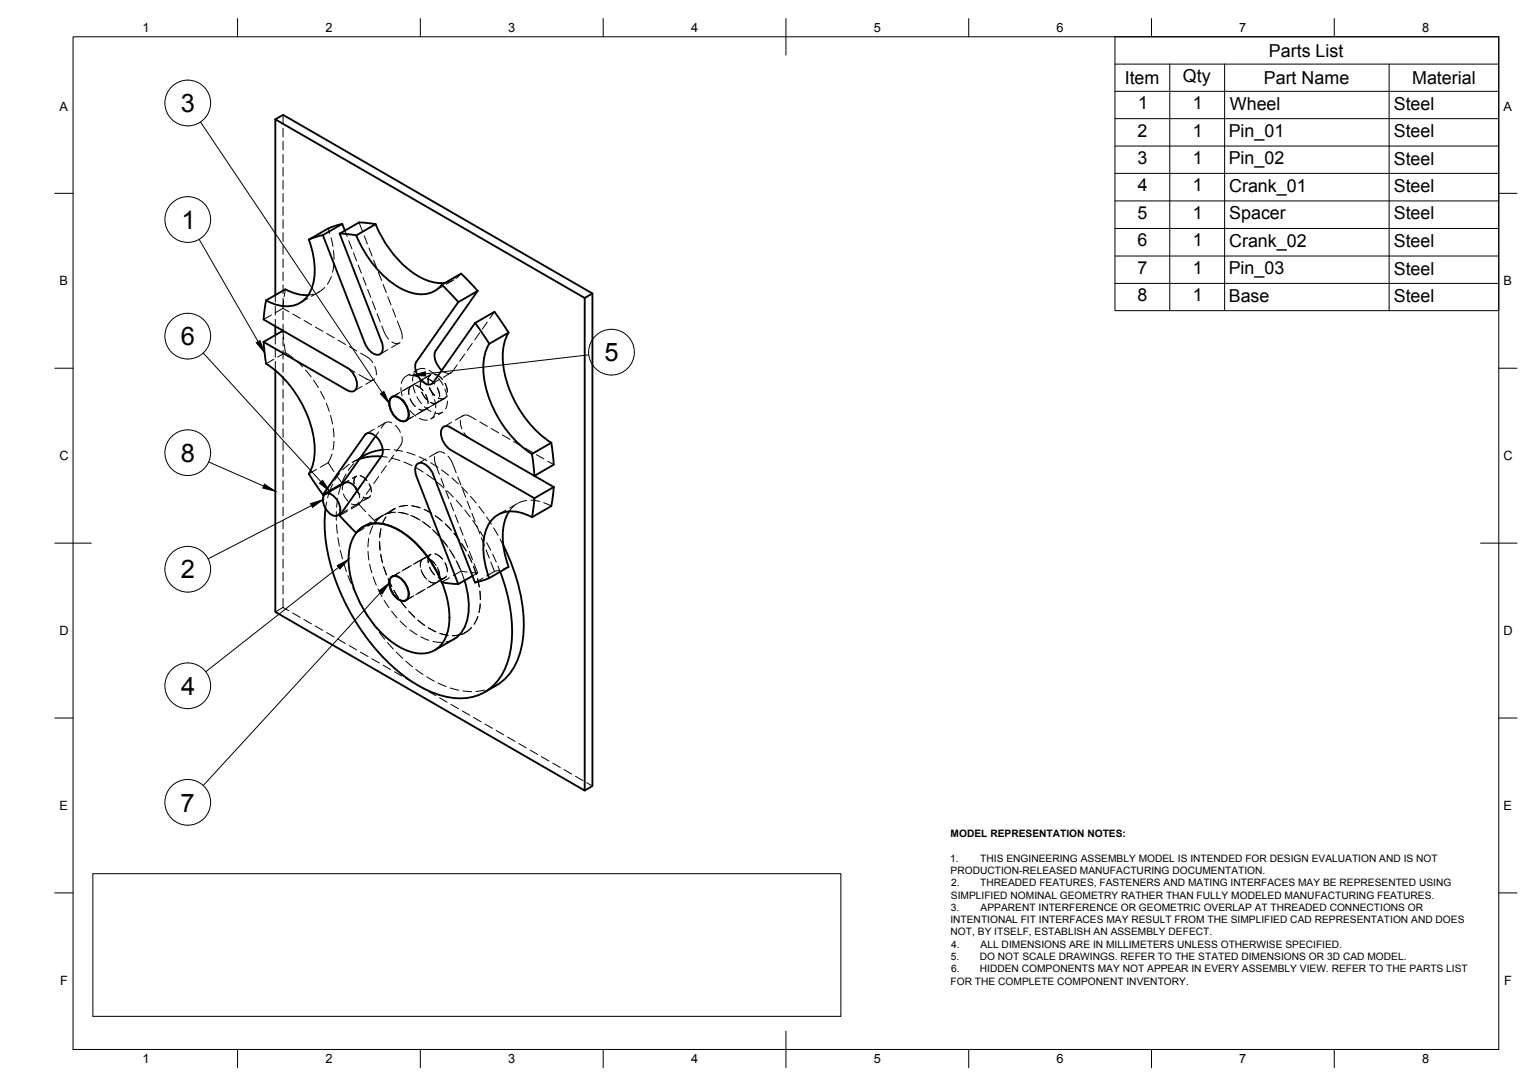
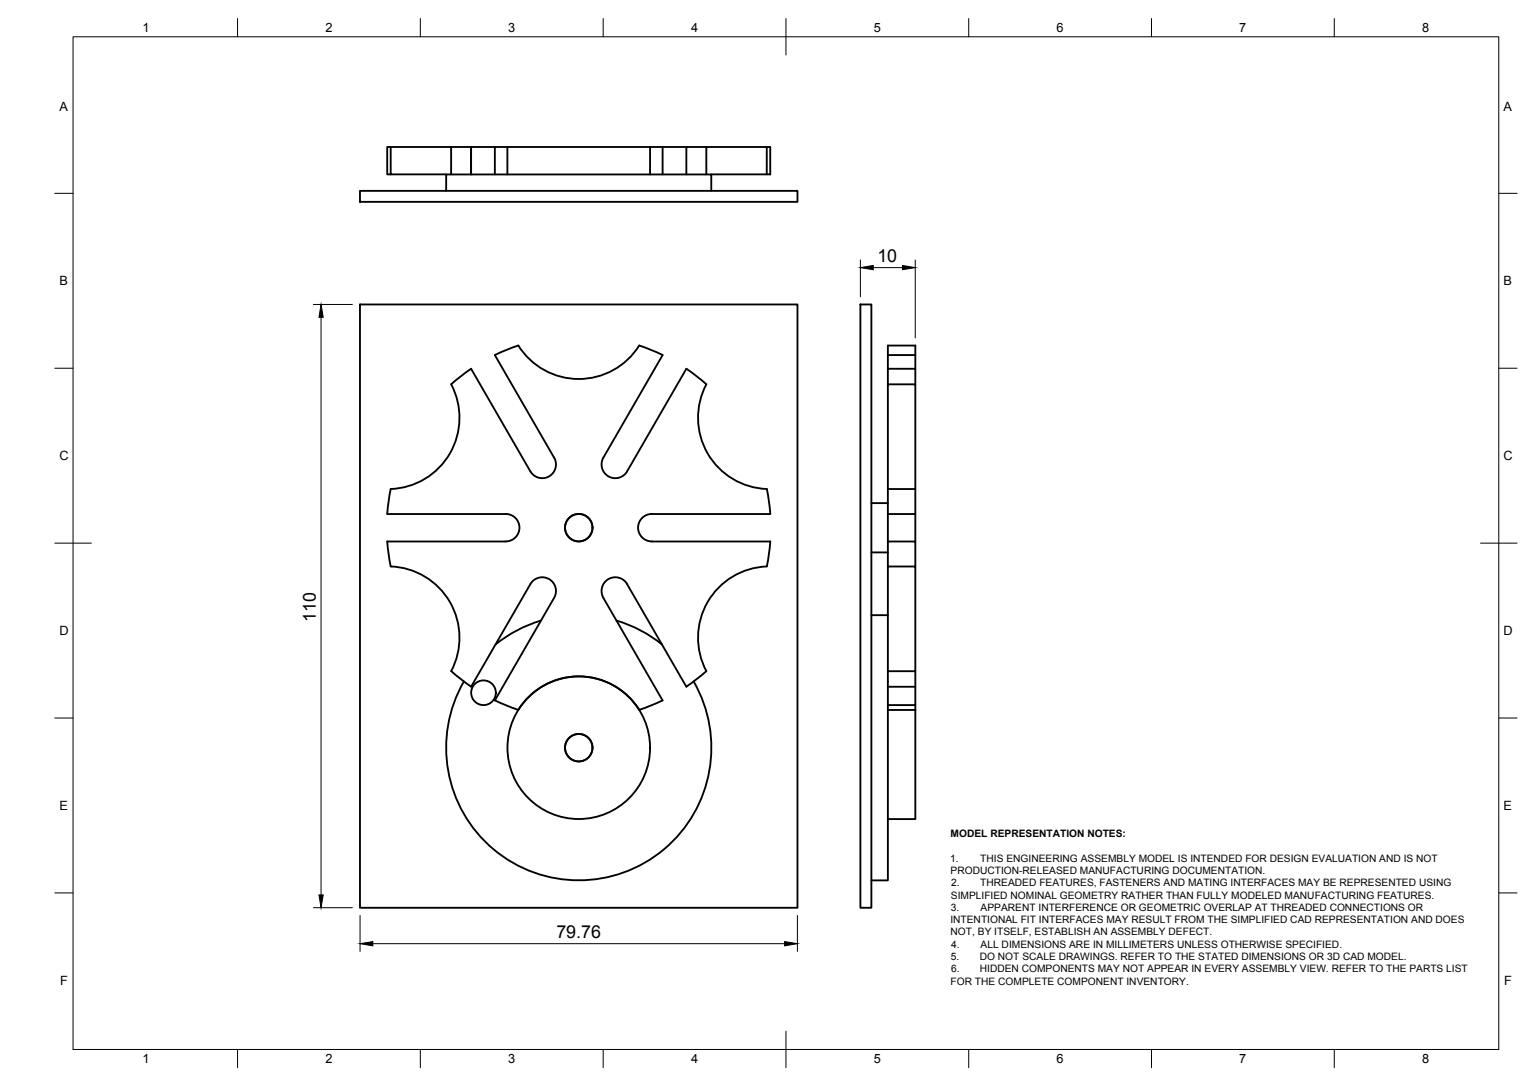
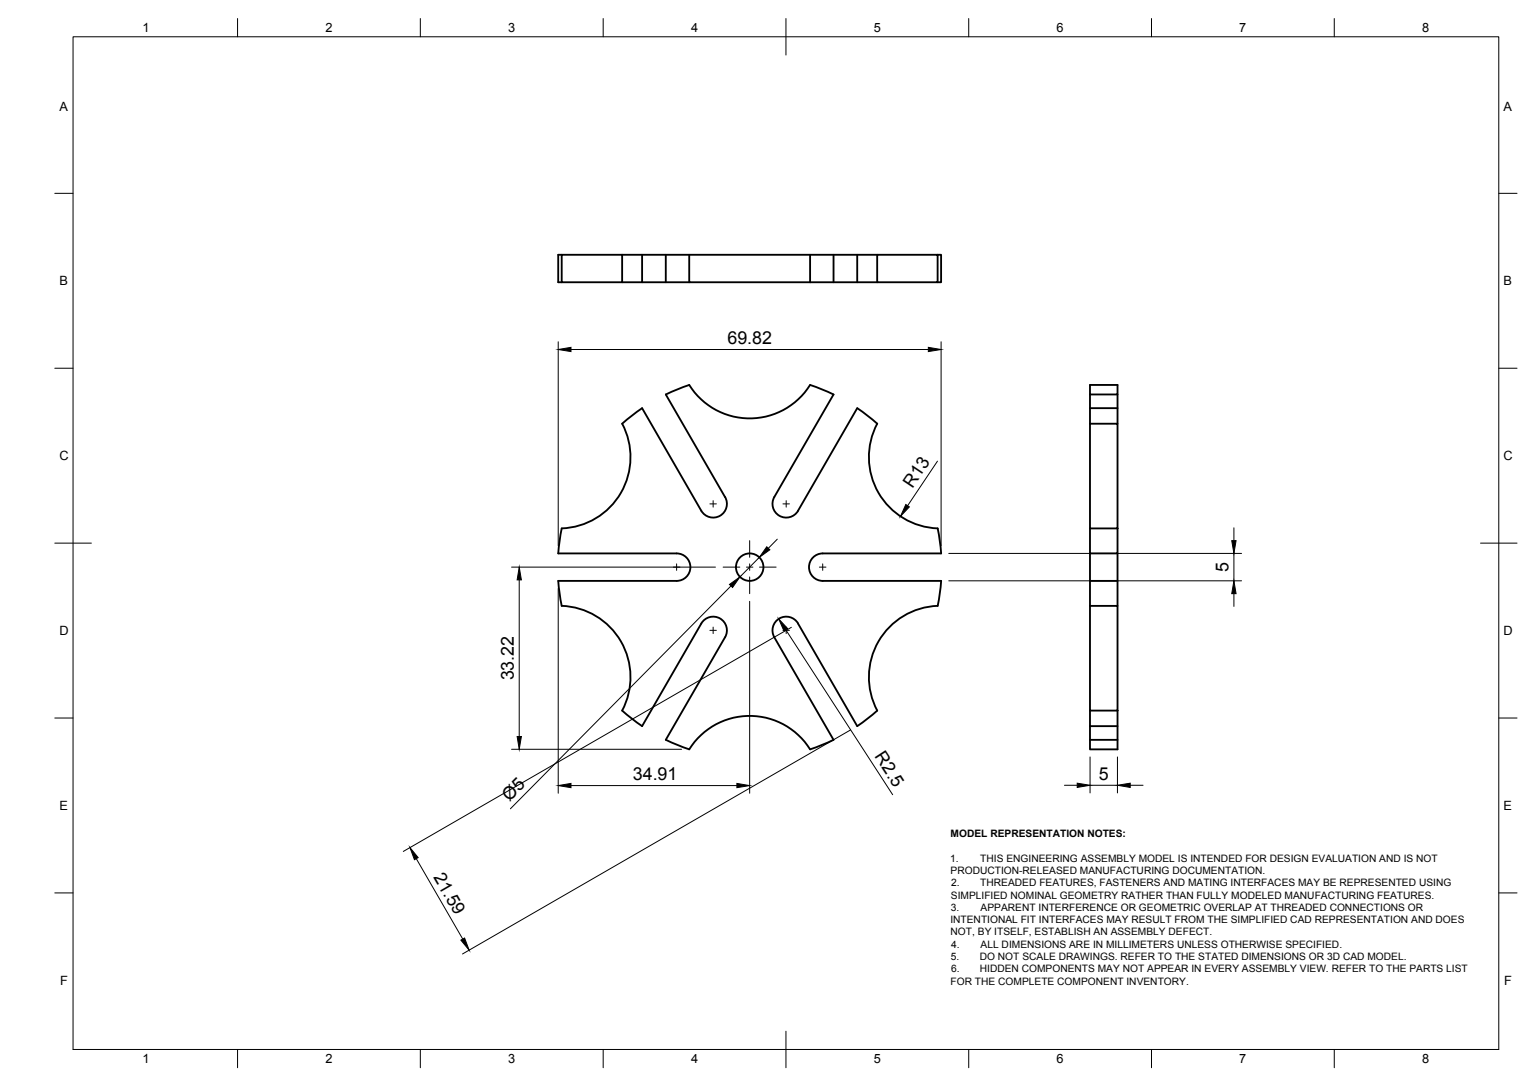
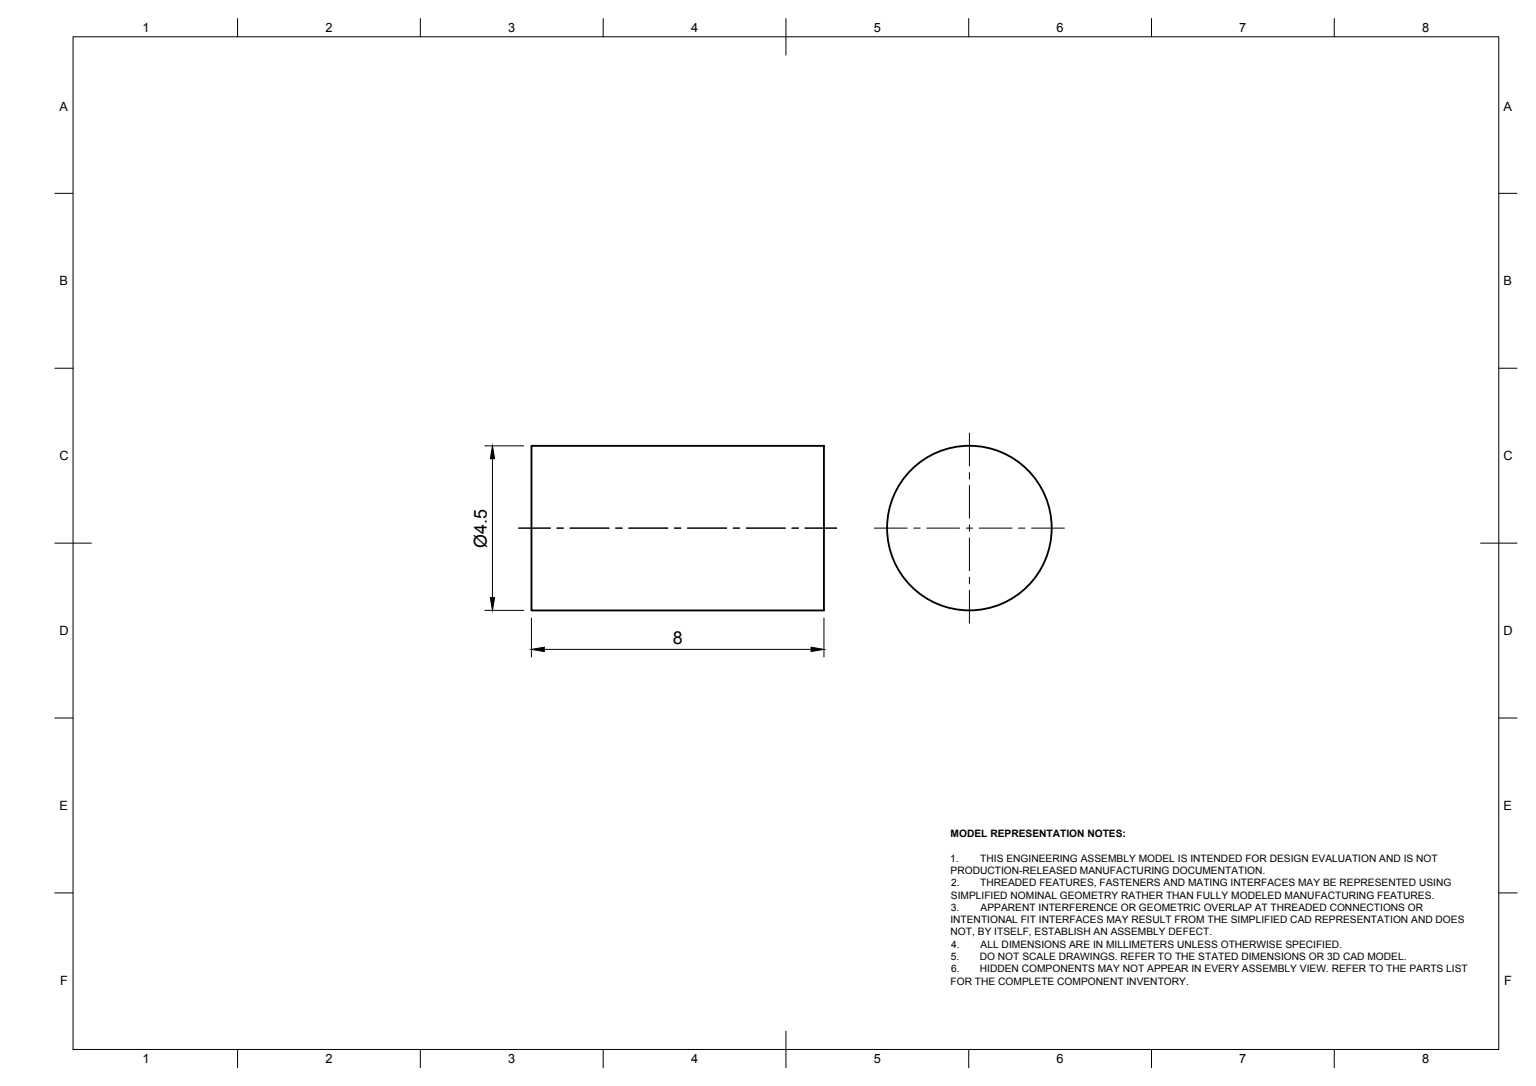
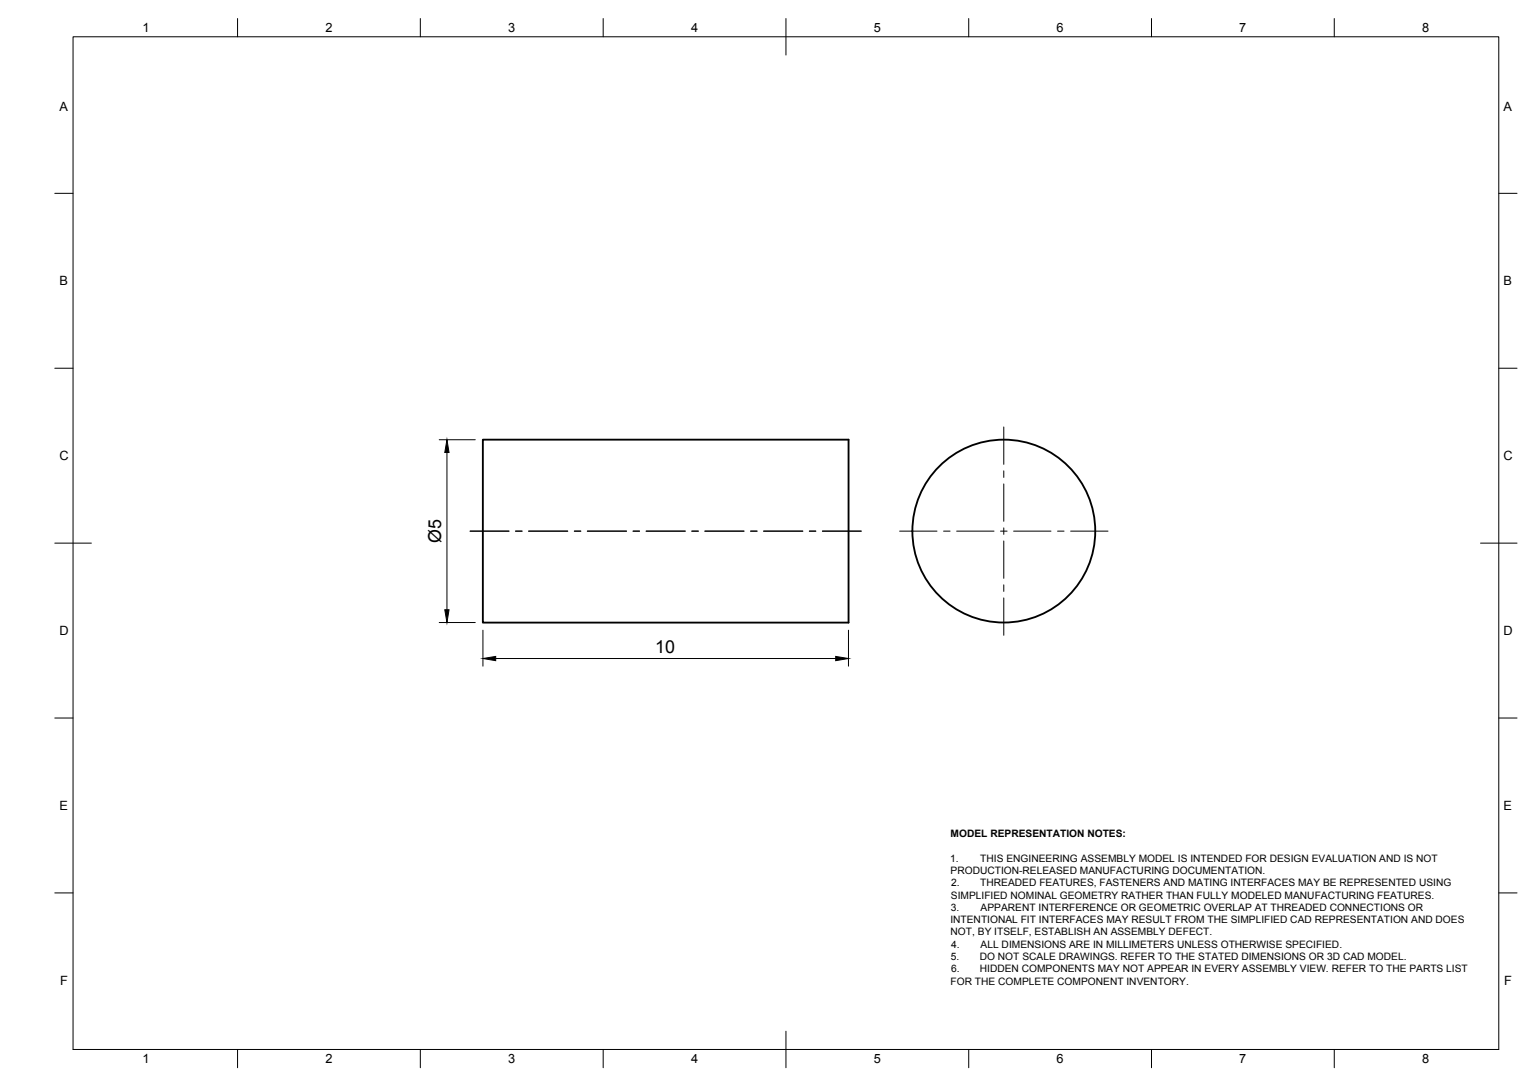
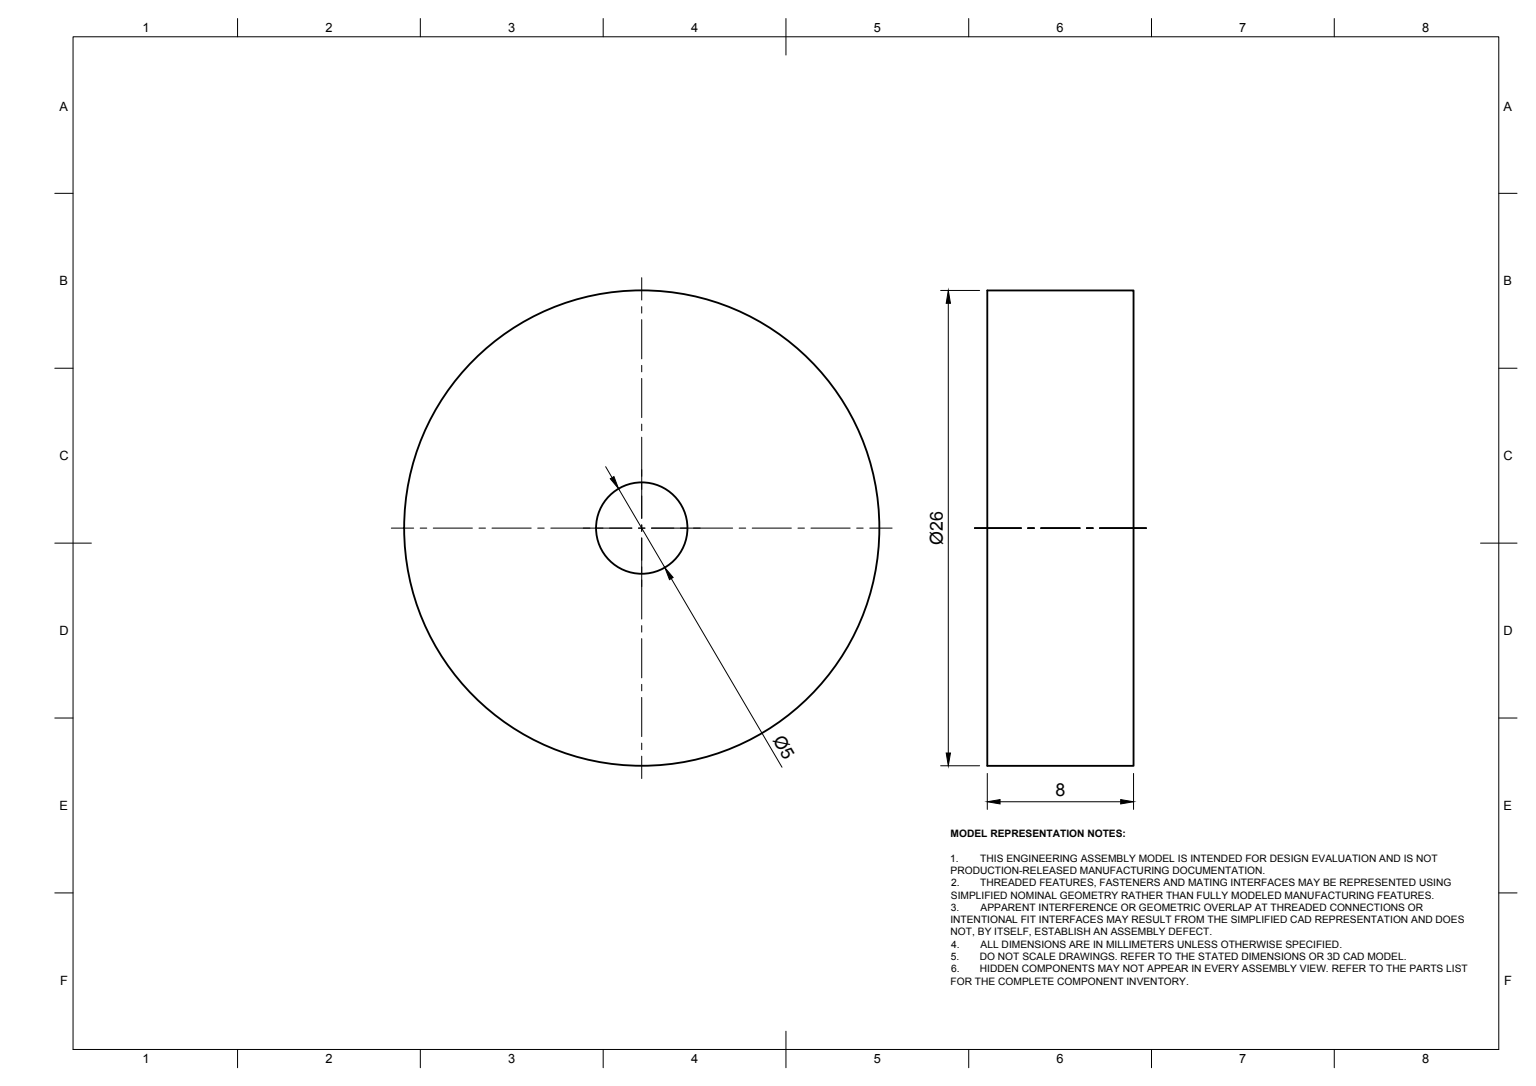
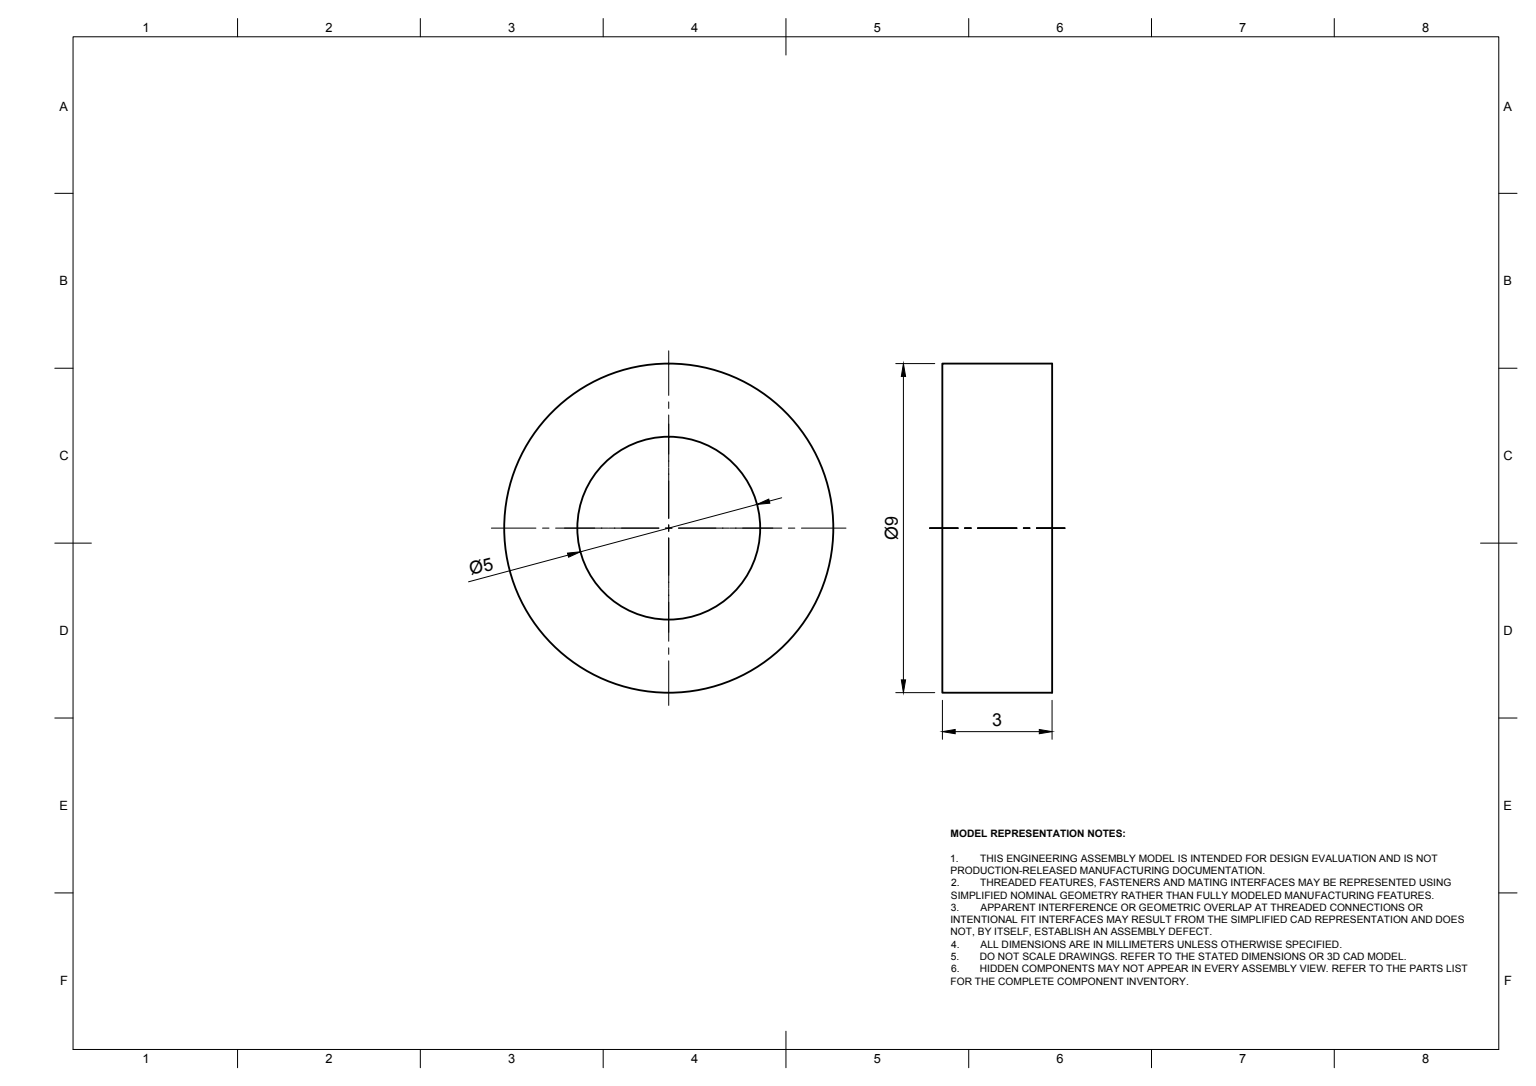
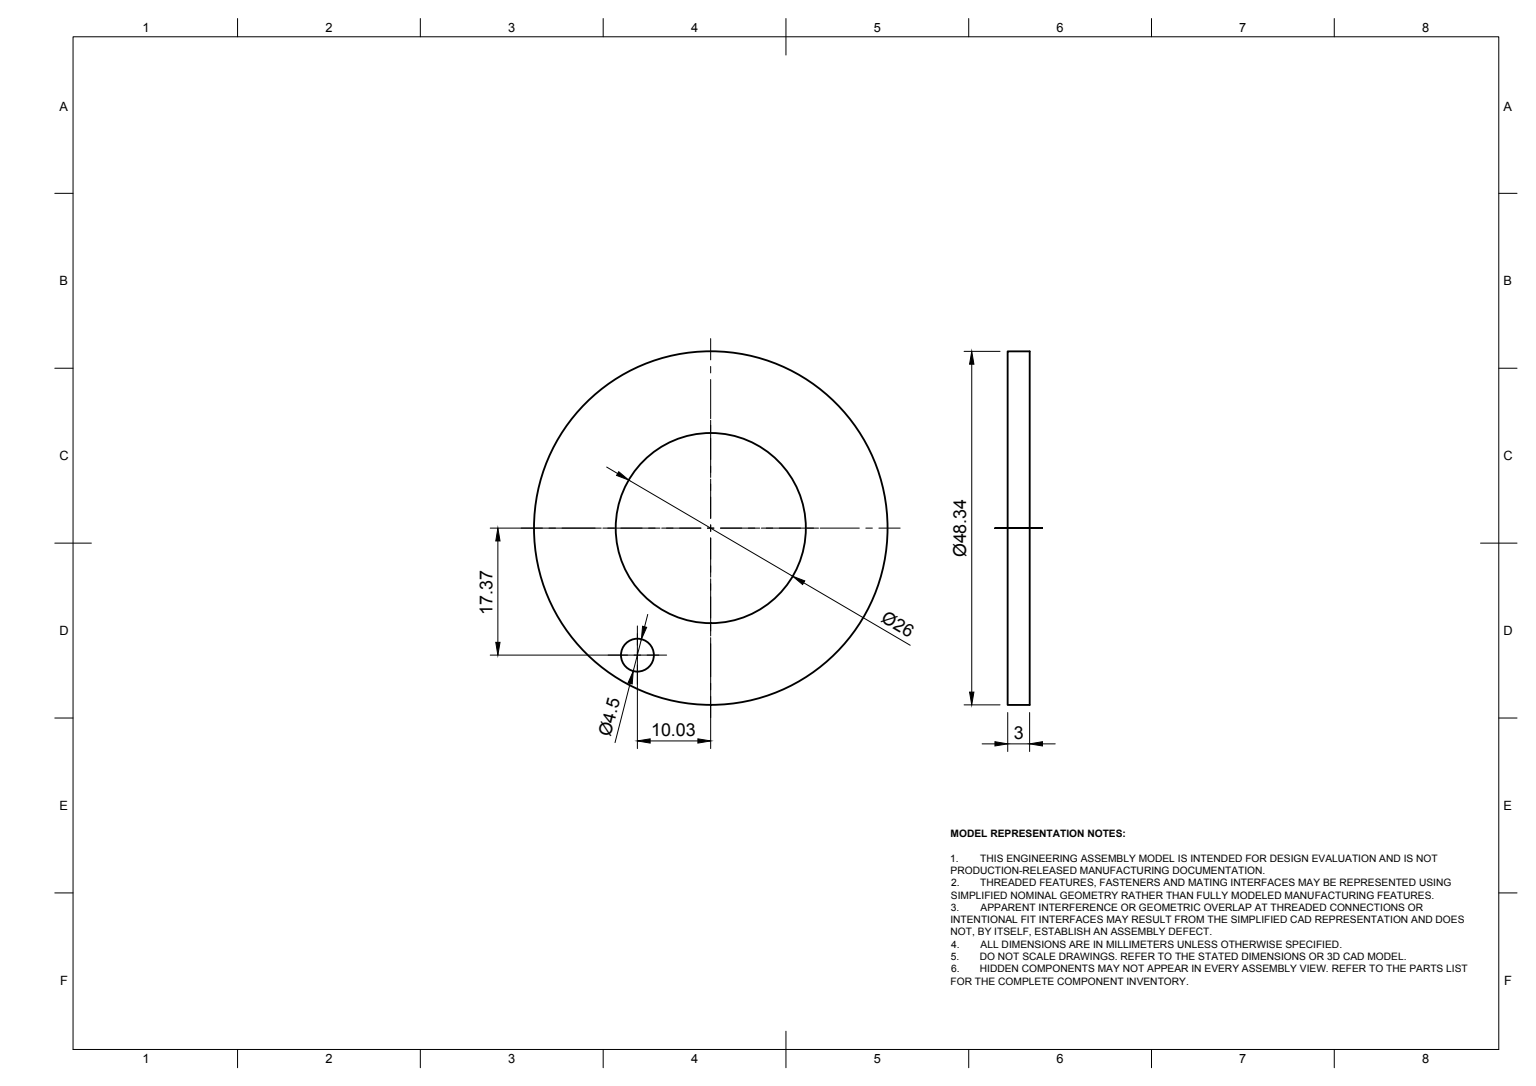
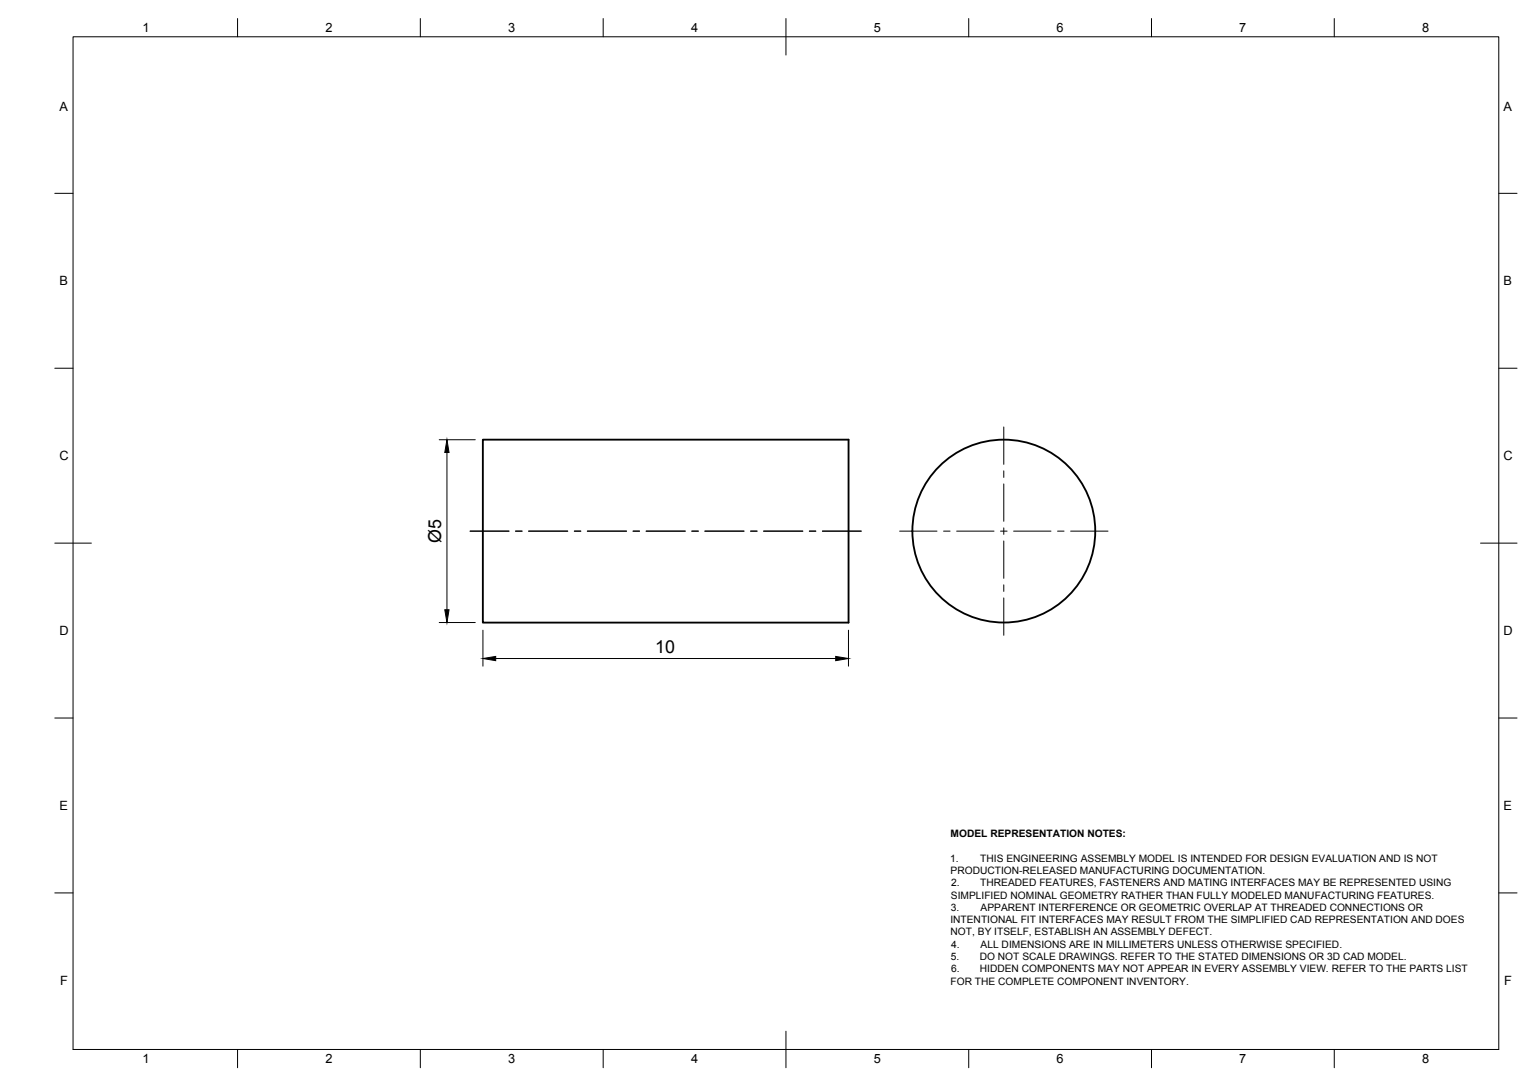
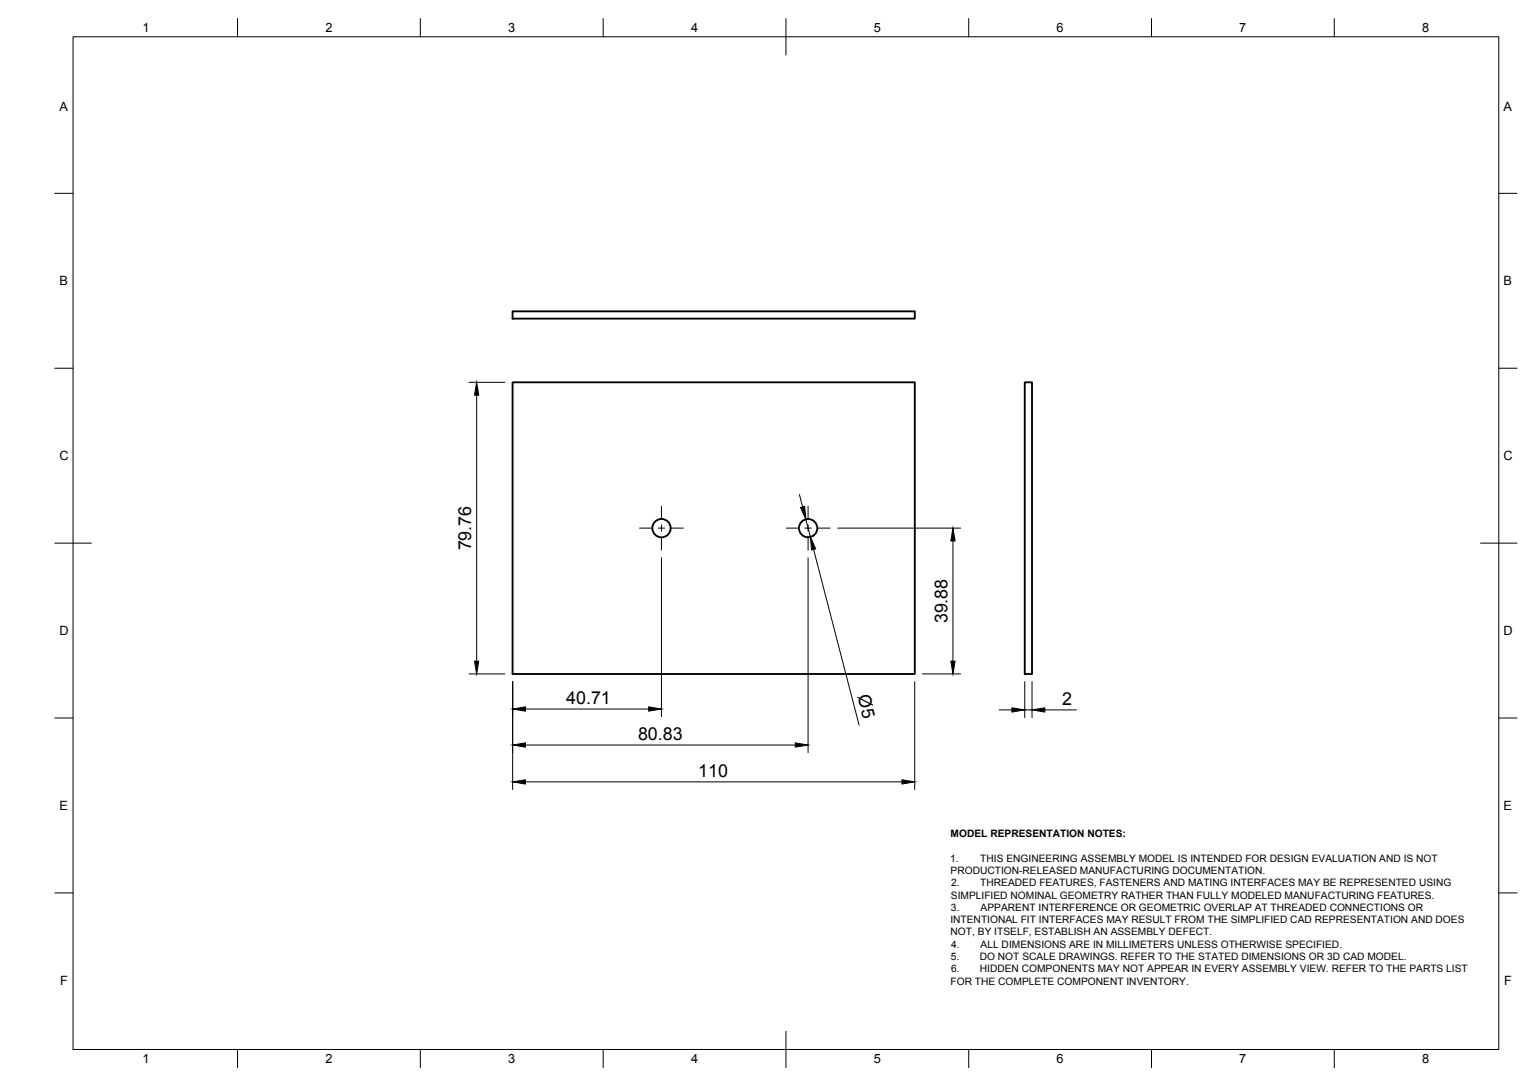
ISO-10303-21;
HEADER;
/* Generated by software containing ST-Developer
 * from STEP Tools, Inc. (www.steptools.com) 
 */

FILE_DESCRIPTION(
/* description */ (''),
/* implementation_level */ '2;1');

FILE_NAME(
/* name */ 'BR-052',
/* time_stamp */ '2026-09-20T21:58:27+06:00',
/* author */ (''),
/* organization */ (''),
/* preprocessor_version */ 'ST-DEVELOPER v20.2',
/* originating_system */ 'Autodesk Translation Framework v15.15.0.0',
/* authorisation */ '');

FILE_SCHEMA (('AUTOMOTIVE_DESIGN { 1 0 10303 214 3 1 1 }'));
ENDSEC;

DATA;
#10=MECHANICAL_DESIGN_GEOMETRIC_PRESENTATION_REPRESENTATION('',(#59,#60,
#61,#62,#63,#64,#65,#66),#2238);
#11=ITEM_DEFINED_TRANSFORMATION($,$,#1304,#1455);
#12=ITEM_DEFINED_TRANSFORMATION($,$,#1394,#1456);
#13=ITEM_DEFINED_TRANSFORMATION($,$,#1400,#1457);
#14=ITEM_DEFINED_TRANSFORMATION($,$,#1406,#1458);
#15=ITEM_DEFINED_TRANSFORMATION($,$,#1415,#1459);
#16=ITEM_DEFINED_TRANSFORMATION($,$,#1424,#1460);
#17=ITEM_DEFINED_TRANSFORMATION($,$,#1436,#1461);
#18=ITEM_DEFINED_TRANSFORMATION($,$,#1442,#1462);
#19=(
REPRESENTATION_RELATIONSHIP($,$,#2270,#2269)
REPRESENTATION_RELATIONSHIP_WITH_TRANSFORMATION(#11)
SHAPE_REPRESENTATION_RELATIONSHIP()
);
#20=(
REPRESENTATION_RELATIONSHIP($,$,#2271,#2269)
REPRESENTATION_RELATIONSHIP_WITH_TRANSFORMATION(#12)
SHAPE_REPRESENTATION_RELATIONSHIP()
);
#21=(
REPRESENTATION_RELATIONSHIP($,$,#2272,#2269)
REPRESENTATION_RELATIONSHIP_WITH_TRANSFORMATION(#13)
SHAPE_REPRESENTATION_RELATIONSHIP()
);
#22=(
REPRESENTATION_RELATIONSHIP($,$,#2273,#2269)
REPRESENTATION_RELATIONSHIP_WITH_TRANSFORMATION(#14)
SHAPE_REPRESENTATION_RELATIONSHIP()
);
#23=(
REPRESENTATION_RELATIONSHIP($,$,#2274,#2269)
REPRESENTATION_RELATIONSHIP_WITH_TRANSFORMATION(#15)
SHAPE_REPRESENTATION_RELATIONSHIP()
);
#24=(
REPRESENTATION_RELATIONSHIP($,$,#2275,#2269)
REPRESENTATION_RELATIONSHIP_WITH_TRANSFORMATION(#16)
SHAPE_REPRESENTATION_RELATIONSHIP()
);
#25=(
REPRESENTATION_RELATIONSHIP($,$,#2276,#2269)
REPRESENTATION_RELATIONSHIP_WITH_TRANSFORMATION(#17)
SHAPE_REPRESENTATION_RELATIONSHIP()
);
#26=(
REPRESENTATION_RELATIONSHIP($,$,#2277,#2269)
REPRESENTATION_RELATIONSHIP_WITH_TRANSFORMATION(#18)
SHAPE_REPRESENTATION_RELATIONSHIP()
);
#27=CONTEXT_DEPENDENT_SHAPE_REPRESENTATION(#19,#2261);
#28=CONTEXT_DEPENDENT_SHAPE_REPRESENTATION(#20,#2262);
#29=CONTEXT_DEPENDENT_SHAPE_REPRESENTATION(#21,#2263);
#30=CONTEXT_DEPENDENT_SHAPE_REPRESENTATION(#22,#2264);
#31=CONTEXT_DEPENDENT_SHAPE_REPRESENTATION(#23,#2265);
#32=CONTEXT_DEPENDENT_SHAPE_REPRESENTATION(#24,#2266);
#33=CONTEXT_DEPENDENT_SHAPE_REPRESENTATION(#25,#2267);
#34=CONTEXT_DEPENDENT_SHAPE_REPRESENTATION(#26,#2268);
#35=NEXT_ASSEMBLY_USAGE_OCCURRENCE('Wheel:1','Wheel:1','Wheel:1',#2279,
#2280,'Wheel:1');
#36=NEXT_ASSEMBLY_USAGE_OCCURRENCE('Pin_01:1','Pin_01:1','Pin_01:1',#2279,
#2281,'Pin_01:1');
#37=NEXT_ASSEMBLY_USAGE_OCCURRENCE('Pin_02:1','Pin_02:1','Pin_02:1',#2279,
#2282,'Pin_02:1');
#38=NEXT_ASSEMBLY_USAGE_OCCURRENCE('Crank_01:1','Crank_01:1',
'Crank_01:1',#2279,#2283,'Crank_01:1');
#39=NEXT_ASSEMBLY_USAGE_OCCURRENCE('Spacer:1','Spacer:1','Spacer:1',#2279,
#2284,'Spacer:1');
#40=NEXT_ASSEMBLY_USAGE_OCCURRENCE('Crank_02:1','Crank_02:1',
'Crank_02:1',#2279,#2285,'Crank_02:1');
#41=NEXT_ASSEMBLY_USAGE_OCCURRENCE('Pin_03:1','Pin_03:1','Pin_03:1',#2279,
#2286,'Pin_03:1');
#42=NEXT_ASSEMBLY_USAGE_OCCURRENCE('Base:1','Base:1','Base:1',#2279,#2287,
'Base:1');
#43=SHAPE_REPRESENTATION_RELATIONSHIP('SRR','None',#2270,#51);
#44=SHAPE_REPRESENTATION_RELATIONSHIP('SRR','None',#2271,#52);
#45=SHAPE_REPRESENTATION_RELATIONSHIP('SRR','None',#2272,#53);
#46=SHAPE_REPRESENTATION_RELATIONSHIP('SRR','None',#2273,#54);
#47=SHAPE_REPRESENTATION_RELATIONSHIP('SRR','None',#2274,#55);
#48=SHAPE_REPRESENTATION_RELATIONSHIP('SRR','None',#2275,#56);
#49=SHAPE_REPRESENTATION_RELATIONSHIP('SRR','None',#2276,#57);
#50=SHAPE_REPRESENTATION_RELATIONSHIP('SRR','None',#2277,#58);
#51=ADVANCED_BREP_SHAPE_REPRESENTATION('',(#67),#2230);
#52=ADVANCED_BREP_SHAPE_REPRESENTATION('',(#68),#2231);
#53=ADVANCED_BREP_SHAPE_REPRESENTATION('',(#69),#2232);
#54=ADVANCED_BREP_SHAPE_REPRESENTATION('',(#70),#2233);
#55=ADVANCED_BREP_SHAPE_REPRESENTATION('',(#71),#2234);
#56=ADVANCED_BREP_SHAPE_REPRESENTATION('',(#72),#2235);
#57=ADVANCED_BREP_SHAPE_REPRESENTATION('',(#73),#2236);
#58=ADVANCED_BREP_SHAPE_REPRESENTATION('',(#74),#2237);
#59=STYLED_ITEM('',(#2319),#67);
#60=STYLED_ITEM('',(#2320),#68);
#61=STYLED_ITEM('',(#2321),#69);
#62=STYLED_ITEM('',(#2320),#70);
#63=STYLED_ITEM('',(#2321),#71);
#64=STYLED_ITEM('',(#2320),#72);
#65=STYLED_ITEM('',(#2321),#73);
#66=STYLED_ITEM('',(#2321),#74);
#67=MANIFOLD_SOLID_BREP('Wheel',#1206);
#68=MANIFOLD_SOLID_BREP('Pin_01',#1207);
#69=MANIFOLD_SOLID_BREP('Pin_02',#1208);
#70=MANIFOLD_SOLID_BREP('Crank_01',#1209);
#71=MANIFOLD_SOLID_BREP('Spacer',#1210);
#72=MANIFOLD_SOLID_BREP('Crank_02',#1211);
#73=MANIFOLD_SOLID_BREP('Pin_03',#1212);
#74=MANIFOLD_SOLID_BREP('Base',#1213);
#75=FACE_BOUND('',#201,.T.);
#76=FACE_BOUND('',#205,.T.);
#77=FACE_BOUND('',#239,.T.);
#78=FACE_BOUND('',#242,.T.);
#79=FACE_BOUND('',#244,.T.);
#80=FACE_BOUND('',#248,.T.);
#81=FACE_BOUND('',#253,.T.);
#82=FACE_BOUND('',#254,.T.);
#83=FACE_BOUND('',#256,.T.);
#84=FACE_BOUND('',#257,.T.);
#85=FACE_BOUND('',#264,.T.);
#86=FACE_BOUND('',#265,.T.);
#87=FACE_BOUND('',#271,.T.);
#88=FACE_BOUND('',#272,.T.);
#89=PLANE('',#1335);
#90=PLANE('',#1355);
#91=PLANE('',#1371);
#92=PLANE('',#1373);
#93=PLANE('',#1375);
#94=PLANE('',#1376);
#95=PLANE('',#1378);
#96=PLANE('',#1380);
#97=PLANE('',#1381);
#98=PLANE('',#1383);
#99=PLANE('',#1385);
#100=PLANE('',#1388);
#101=PLANE('',#1390);
#102=PLANE('',#1392);
#103=PLANE('',#1395);
#104=PLANE('',#1399);
#105=PLANE('',#1401);
#106=PLANE('',#1405);
#107=PLANE('',#1410);
#108=PLANE('',#1414);
#109=PLANE('',#1416);
#110=PLANE('',#1423);
#111=PLANE('',#1434);
#112=PLANE('',#1435);
#113=PLANE('',#1437);
#114=PLANE('',#1441);
#115=PLANE('',#1449);
#116=PLANE('',#1450);
#117=PLANE('',#1451);
#118=PLANE('',#1452);
#119=PLANE('',#1453);
#120=PLANE('',#1454);
#121=FACE_OUTER_BOUND('',#190,.T.);
#122=FACE_OUTER_BOUND('',#191,.T.);
#123=FACE_OUTER_BOUND('',#192,.T.);
#124=FACE_OUTER_BOUND('',#193,.T.);
#125=FACE_OUTER_BOUND('',#194,.T.);
#126=FACE_OUTER_BOUND('',#195,.T.);
#127=FACE_OUTER_BOUND('',#196,.T.);
#128=FACE_OUTER_BOUND('',#197,.T.);
#129=FACE_OUTER_BOUND('',#198,.T.);
#130=FACE_OUTER_BOUND('',#199,.T.);
#131=FACE_OUTER_BOUND('',#200,.T.);
#132=FACE_OUTER_BOUND('',#202,.T.);
#133=FACE_OUTER_BOUND('',#203,.T.);
#134=FACE_OUTER_BOUND('',#204,.T.);
#135=FACE_OUTER_BOUND('',#206,.T.);
#136=FACE_OUTER_BOUND('',#207,.T.);
#137=FACE_OUTER_BOUND('',#208,.T.);
#138=FACE_OUTER_BOUND('',#209,.T.);
#139=FACE_OUTER_BOUND('',#210,.T.);
#140=FACE_OUTER_BOUND('',#211,.T.);
#141=FACE_OUTER_BOUND('',#212,.T.);
#142=FACE_OUTER_BOUND('',#213,.T.);
#143=FACE_OUTER_BOUND('',#214,.T.);
#144=FACE_OUTER_BOUND('',#215,.T.);
#145=FACE_OUTER_BOUND('',#216,.T.);
#146=FACE_OUTER_BOUND('',#217,.T.);
#147=FACE_OUTER_BOUND('',#218,.T.);
#148=FACE_OUTER_BOUND('',#219,.T.);
#149=FACE_OUTER_BOUND('',#220,.T.);
#150=FACE_OUTER_BOUND('',#221,.T.);
#151=FACE_OUTER_BOUND('',#222,.T.);
#152=FACE_OUTER_BOUND('',#223,.T.);
#153=FACE_OUTER_BOUND('',#224,.T.);
#154=FACE_OUTER_BOUND('',#225,.T.);
#155=FACE_OUTER_BOUND('',#226,.T.);
#156=FACE_OUTER_BOUND('',#227,.T.);
#157=FACE_OUTER_BOUND('',#228,.T.);
#158=FACE_OUTER_BOUND('',#229,.T.);
#159=FACE_OUTER_BOUND('',#230,.T.);
#160=FACE_OUTER_BOUND('',#231,.T.);
#161=FACE_OUTER_BOUND('',#232,.T.);
#162=FACE_OUTER_BOUND('',#233,.T.);
#163=FACE_OUTER_BOUND('',#234,.T.);
#164=FACE_OUTER_BOUND('',#235,.T.);
#165=FACE_OUTER_BOUND('',#236,.T.);
#166=FACE_OUTER_BOUND('',#237,.T.);
#167=FACE_OUTER_BOUND('',#238,.T.);
#168=FACE_OUTER_BOUND('',#240,.T.);
#169=FACE_OUTER_BOUND('',#241,.T.);
#170=FACE_OUTER_BOUND('',#243,.T.);
#171=FACE_OUTER_BOUND('',#245,.T.);
#172=FACE_OUTER_BOUND('',#246,.T.);
#173=FACE_OUTER_BOUND('',#247,.T.);
#174=FACE_OUTER_BOUND('',#249,.T.);
#175=FACE_OUTER_BOUND('',#250,.T.);
#176=FACE_OUTER_BOUND('',#251,.T.);
#177=FACE_OUTER_BOUND('',#252,.T.);
#178=FACE_OUTER_BOUND('',#255,.T.);
#179=FACE_OUTER_BOUND('',#258,.T.);
#180=FACE_OUTER_BOUND('',#259,.T.);
#181=FACE_OUTER_BOUND('',#260,.T.);
#182=FACE_OUTER_BOUND('',#261,.T.);
#183=FACE_OUTER_BOUND('',#262,.T.);
#184=FACE_OUTER_BOUND('',#263,.T.);
#185=FACE_OUTER_BOUND('',#266,.T.);
#186=FACE_OUTER_BOUND('',#267,.T.);
#187=FACE_OUTER_BOUND('',#268,.T.);
#188=FACE_OUTER_BOUND('',#269,.T.);
#189=FACE_OUTER_BOUND('',#270,.T.);
#190=EDGE_LOOP('',(#782,#783,#784,#785));
#191=EDGE_LOOP('',(#786,#787,#788,#789));
#192=EDGE_LOOP('',(#790,#791,#792,#793));
#193=EDGE_LOOP('',(#794,#795,#796,#797));
#194=EDGE_LOOP('',(#798,#799,#800,#801));
#195=EDGE_LOOP('',(#802,#803,#804,#805));
#196=EDGE_LOOP('',(#806,#807,#808,#809));
#197=EDGE_LOOP('',(#810,#811,#812,#813));
#198=EDGE_LOOP('',(#814,#815,#816,#817));
#199=EDGE_LOOP('',(#818,#819,#820,#821));
#200=EDGE_LOOP('',(#822,#823,#824,#825,#826,#827,#828,#829,#830,#831,#832,
#833,#834,#835,#836,#837,#838,#839,#840,#841,#842,#843,#844,#845,#846,#847,
#848,#849,#850,#851,#852,#853,#854,#855,#856,#857));
#201=EDGE_LOOP('',(#858));
#202=EDGE_LOOP('',(#859,#860,#861,#862));
#203=EDGE_LOOP('',(#863,#864,#865,#866));
#204=EDGE_LOOP('',(#867,#868,#869,#870,#871,#872,#873,#874,#875,#876,#877,
#878,#879,#880,#881,#882,#883,#884,#885,#886,#887,#888,#889,#890,#891,#892,
#893,#894,#895,#896,#897,#898,#899,#900,#901,#902));
#205=EDGE_LOOP('',(#903));
#206=EDGE_LOOP('',(#904,#905,#906,#907));
#207=EDGE_LOOP('',(#908,#909,#910,#911));
#208=EDGE_LOOP('',(#912,#913,#914,#915));
#209=EDGE_LOOP('',(#916,#917,#918,#919));
#210=EDGE_LOOP('',(#920,#921,#922,#923));
#211=EDGE_LOOP('',(#924,#925,#926,#927));
#212=EDGE_LOOP('',(#928,#929,#930,#931));
#213=EDGE_LOOP('',(#932,#933,#934,#935));
#214=EDGE_LOOP('',(#936,#937,#938,#939));
#215=EDGE_LOOP('',(#940,#941,#942,#943));
#216=EDGE_LOOP('',(#944,#945,#946,#947));
#217=EDGE_LOOP('',(#948,#949,#950,#951));
#218=EDGE_LOOP('',(#952,#953,#954,#955));
#219=EDGE_LOOP('',(#956,#957,#958,#959));
#220=EDGE_LOOP('',(#960,#961,#962,#963));
#221=EDGE_LOOP('',(#964,#965,#966,#967));
#222=EDGE_LOOP('',(#968,#969,#970,#971));
#223=EDGE_LOOP('',(#972,#973,#974,#975));
#224=EDGE_LOOP('',(#976,#977,#978,#979));
#225=EDGE_LOOP('',(#980,#981,#982,#983));
#226=EDGE_LOOP('',(#984,#985,#986,#987));
#227=EDGE_LOOP('',(#988,#989,#990,#991));
#228=EDGE_LOOP('',(#992,#993,#994,#995));
#229=EDGE_LOOP('',(#996,#997,#998,#999));
#230=EDGE_LOOP('',(#1000,#1001,#1002,#1003));
#231=EDGE_LOOP('',(#1004));
#232=EDGE_LOOP('',(#1005,#1006,#1007,#1008));
#233=EDGE_LOOP('',(#1009));
#234=EDGE_LOOP('',(#1010));
#235=EDGE_LOOP('',(#1011,#1012,#1013,#1014));
#236=EDGE_LOOP('',(#1015));
#237=EDGE_LOOP('',(#1016,#1017,#1018,#1019));
#238=EDGE_LOOP('',(#1020));
#239=EDGE_LOOP('',(#1021));
#240=EDGE_LOOP('',(#1022,#1023,#1024,#1025));
#241=EDGE_LOOP('',(#1026));
#242=EDGE_LOOP('',(#1027));
#243=EDGE_LOOP('',(#1028));
#244=EDGE_LOOP('',(#1029));
#245=EDGE_LOOP('',(#1030,#1031,#1032,#1033));
#246=EDGE_LOOP('',(#1034,#1035,#1036,#1037));
#247=EDGE_LOOP('',(#1038));
#248=EDGE_LOOP('',(#1039));
#249=EDGE_LOOP('',(#1040,#1041,#1042,#1043));
#250=EDGE_LOOP('',(#1044,#1045,#1046,#1047));
#251=EDGE_LOOP('',(#1048,#1049,#1050,#1051));
#252=EDGE_LOOP('',(#1052));
#253=EDGE_LOOP('',(#1053));
#254=EDGE_LOOP('',(#1054));
#255=EDGE_LOOP('',(#1055));
#256=EDGE_LOOP('',(#1056));
#257=EDGE_LOOP('',(#1057));
#258=EDGE_LOOP('',(#1058));
#259=EDGE_LOOP('',(#1059,#1060,#1061,#1062));
#260=EDGE_LOOP('',(#1063));
#261=EDGE_LOOP('',(#1064,#1065,#1066,#1067));
#262=EDGE_LOOP('',(#1068,#1069,#1070,#1071));
#263=EDGE_LOOP('',(#1072,#1073,#1074,#1075));
#264=EDGE_LOOP('',(#1076));
#265=EDGE_LOOP('',(#1077));
#266=EDGE_LOOP('',(#1078,#1079,#1080,#1081));
#267=EDGE_LOOP('',(#1082,#1083,#1084,#1085));
#268=EDGE_LOOP('',(#1086,#1087,#1088,#1089));
#269=EDGE_LOOP('',(#1090,#1091,#1092,#1093));
#270=EDGE_LOOP('',(#1094,#1095,#1096,#1097));
#271=EDGE_LOOP('',(#1098));
#272=EDGE_LOOP('',(#1099));
#273=LINE('',#1874,#358);
#274=LINE('',#1879,#359);
#275=LINE('',#1883,#360);
#276=LINE('',#1888,#361);
#277=LINE('',#1892,#362);
#278=LINE('',#1897,#363);
#279=LINE('',#1901,#364);
#280=LINE('',#1906,#365);
#281=LINE('',#1910,#366);
#282=LINE('',#1915,#367);
#283=LINE('',#1919,#368);
#284=LINE('',#1925,#369);
#285=LINE('',#1931,#370);
#286=LINE('',#1937,#371);
#287=LINE('',#1943,#372);
#288=LINE('',#1947,#373);
#289=LINE('',#1951,#374);
#290=LINE('',#1954,#375);
#291=LINE('',#1958,#376);
#292=LINE('',#1961,#377);
#293=LINE('',#1965,#378);
#294=LINE('',#1968,#379);
#295=LINE('',#1972,#380);
#296=LINE('',#1977,#381);
#297=LINE('',#1981,#382);
#298=LINE('',#1989,#383);
#299=LINE('',#1993,#384);
#300=LINE('',#1998,#385);
#301=LINE('',#2001,#386);
#302=LINE('',#2003,#387);
#303=LINE('',#2009,#388);
#304=LINE('',#2013,#389);
#305=LINE('',#2018,#390);
#306=LINE('',#2021,#391);
#307=LINE('',#2025,#392);
#308=LINE('',#2028,#393);
#309=LINE('',#2032,#394);
#310=LINE('',#2035,#395);
#311=LINE('',#2039,#396);
#312=LINE('',#2042,#397);
#313=LINE('',#2046,#398);
#314=LINE('',#2049,#399);
#315=LINE('',#2051,#400);
#316=LINE('',#2053,#401);
#317=LINE('',#2055,#402);
#318=LINE('',#2057,#403);
#319=LINE('',#2059,#404);
#320=LINE('',#2062,#405);
#321=LINE('',#2064,#406);
#322=LINE('',#2066,#407);
#323=LINE('',#2069,#408);
#324=LINE('',#2071,#409);
#325=LINE('',#2073,#410);
#326=LINE('',#2074,#411);
#327=LINE('',#2076,#412);
#328=LINE('',#2079,#413);
#329=LINE('',#2081,#414);
#330=LINE('',#2085,#415);
#331=LINE('',#2087,#416);
#332=LINE('',#2089,#417);
#333=LINE('',#2092,#418);
#334=LINE('',#2100,#419);
#335=LINE('',#2109,#420);
#336=LINE('',#2117,#421);
#337=LINE('',#2124,#422);
#338=LINE('',#2135,#423);
#339=LINE('',#2140,#424);
#340=LINE('',#2147,#425);
#341=LINE('',#2153,#426);
#342=LINE('',#2159,#427);
#343=LINE('',#2169,#428);
#344=LINE('',#2177,#429);
#345=LINE('',#2183,#430);
#346=LINE('',#2188,#431);
#347=LINE('',#2190,#432);
#348=LINE('',#2192,#433);
#349=LINE('',#2193,#434);
#350=LINE('',#2196,#435);
#351=LINE('',#2198,#436);
#352=LINE('',#2199,#437);
#353=LINE('',#2202,#438);
#354=LINE('',#2203,#439);
#355=LINE('',#2206,#440);
#356=LINE('',#2207,#441);
#357=LINE('',#2209,#442);
#358=VECTOR('',#1471,2.5);
#359=VECTOR('',#1476,10.);
#360=VECTOR('',#1479,10.);
#361=VECTOR('',#1484,10.);
#362=VECTOR('',#1487,10.);
#363=VECTOR('',#1492,10.);
#364=VECTOR('',#1495,10.);
#365=VECTOR('',#1500,10.);
#366=VECTOR('',#1503,10.);
#367=VECTOR('',#1508,10.);
#368=VECTOR('',#1511,10.);
#369=VECTOR('',#1518,10.);
#370=VECTOR('',#1525,10.);
#371=VECTOR('',#1532,10.);
#372=VECTOR('',#1539,10.);
#373=VECTOR('',#1544,10.);
#374=VECTOR('',#1547,10.);
#375=VECTOR('',#1550,10.);
#376=VECTOR('',#1553,10.);
#377=VECTOR('',#1556,10.);
#378=VECTOR('',#1559,10.);
#379=VECTOR('',#1562,10.);
#380=VECTOR('',#1565,10.);
#381=VECTOR('',#1570,10.);
#382=VECTOR('',#1573,10.);
#383=VECTOR('',#1580,10.);
#384=VECTOR('',#1583,10.);
#385=VECTOR('',#1590,10.);
#386=VECTOR('',#1593,10.);
#387=VECTOR('',#1594,10.);
#388=VECTOR('',#1601,10.);
#389=VECTOR('',#1604,10.);
#390=VECTOR('',#1609,10.);
#391=VECTOR('',#1612,10.);
#392=VECTOR('',#1615,10.);
#393=VECTOR('',#1618,10.);
#394=VECTOR('',#1621,10.);
#395=VECTOR('',#1624,10.);
#396=VECTOR('',#1627,10.);
#397=VECTOR('',#1630,10.);
#398=VECTOR('',#1633,10.);
#399=VECTOR('',#1636,10.);
#400=VECTOR('',#1639,10.);
#401=VECTOR('',#1642,10.);
#402=VECTOR('',#1645,10.);
#403=VECTOR('',#1648,10.);
#404=VECTOR('',#1651,10.);
#405=VECTOR('',#1656,10.);
#406=VECTOR('',#1659,10.);
#407=VECTOR('',#1662,10.);
#408=VECTOR('',#1667,10.);
#409=VECTOR('',#1670,10.);
#410=VECTOR('',#1673,10.);
#411=VECTOR('',#1674,10.);
#412=VECTOR('',#1677,10.);
#413=VECTOR('',#1682,10.);
#414=VECTOR('',#1685,10.);
#415=VECTOR('',#1692,10.);
#416=VECTOR('',#1695,10.);
#417=VECTOR('',#1698,10.);
#418=VECTOR('',#1703,10.);
#419=VECTOR('',#1714,2.25);
#420=VECTOR('',#1727,2.5);
#421=VECTOR('',#1738,2.5);
#422=VECTOR('',#1747,13.);
#423=VECTOR('',#1762,4.5);
#424=VECTOR('',#1769,2.5);
#425=VECTOR('',#1778,13.);
#426=VECTOR('',#1785,2.25);
#427=VECTOR('',#1792,24.1717785126239);
#428=VECTOR('',#1807,2.5);
#429=VECTOR('',#1818,2.5);
#430=VECTOR('',#1825,2.5);
#431=VECTOR('',#1830,10.);
#432=VECTOR('',#1831,10.);
#433=VECTOR('',#1832,10.);
#434=VECTOR('',#1833,10.);
#435=VECTOR('',#1836,10.);
#436=VECTOR('',#1837,10.);
#437=VECTOR('',#1838,10.);
#438=VECTOR('',#1841,10.);
#439=VECTOR('',#1842,10.);
#440=VECTOR('',#1845,10.);
#441=VECTOR('',#1846,10.);
#442=VECTOR('',#1849,10.);
#443=CIRCLE('',#1306,2.5);
#444=CIRCLE('',#1307,2.5);
#445=CIRCLE('',#1309,13.);
#446=CIRCLE('',#1310,13.);
#447=CIRCLE('',#1312,13.);
#448=CIRCLE('',#1313,13.);
#449=CIRCLE('',#1315,13.);
#450=CIRCLE('',#1316,13.);
#451=CIRCLE('',#1318,13.);
#452=CIRCLE('',#1319,13.);
#453=CIRCLE('',#1321,13.);
#454=CIRCLE('',#1322,13.);
#455=CIRCLE('',#1324,35.);
#456=CIRCLE('',#1325,35.);
#457=CIRCLE('',#1327,35.);
#458=CIRCLE('',#1328,35.);
#459=CIRCLE('',#1330,35.);
#460=CIRCLE('',#1331,35.);
#461=CIRCLE('',#1333,35.);
#462=CIRCLE('',#1334,35.);
#463=CIRCLE('',#1336,2.5);
#464=CIRCLE('',#1337,35.);
#465=CIRCLE('',#1338,2.5);
#466=CIRCLE('',#1339,35.);
#467=CIRCLE('',#1340,2.5);
#468=CIRCLE('',#1341,35.);
#469=CIRCLE('',#1342,2.5);
#470=CIRCLE('',#1343,35.);
#471=CIRCLE('',#1344,35.);
#472=CIRCLE('',#1345,2.5);
#473=CIRCLE('',#1346,35.);
#474=CIRCLE('',#1347,13.);
#475=CIRCLE('',#1348,35.);
#476=CIRCLE('',#1349,2.5);
#477=CIRCLE('',#1350,35.);
#478=CIRCLE('',#1352,35.);
#479=CIRCLE('',#1354,13.);
#480=CIRCLE('',#1356,35.);
#481=CIRCLE('',#1357,2.5);
#482=CIRCLE('',#1358,35.);
#483=CIRCLE('',#1359,35.);
#484=CIRCLE('',#1360,2.5);
#485=CIRCLE('',#1361,35.);
#486=CIRCLE('',#1362,2.5);
#487=CIRCLE('',#1363,35.);
#488=CIRCLE('',#1364,2.5);
#489=CIRCLE('',#1365,35.);
#490=CIRCLE('',#1366,2.5);
#491=CIRCLE('',#1367,35.);
#492=CIRCLE('',#1368,2.5);
#493=CIRCLE('',#1396,2.25);
#494=CIRCLE('',#1398,2.25);
#495=CIRCLE('',#1402,2.5);
#496=CIRCLE('',#1404,2.5);
#497=CIRCLE('',#1408,2.5);
#498=CIRCLE('',#1409,2.5);
#499=CIRCLE('',#1411,13.);
#500=CIRCLE('',#1413,13.);
#501=CIRCLE('',#1417,4.5);
#502=CIRCLE('',#1418,2.5);
#503=CIRCLE('',#1420,4.5);
#504=CIRCLE('',#1422,2.5);
#505=CIRCLE('',#1426,13.);
#506=CIRCLE('',#1427,13.);
#507=CIRCLE('',#1429,2.25);
#508=CIRCLE('',#1430,2.25);
#509=CIRCLE('',#1432,24.1717785126239);
#510=CIRCLE('',#1433,24.1717785126239);
#511=CIRCLE('',#1438,2.5);
#512=CIRCLE('',#1440,2.5);
#513=CIRCLE('',#1444,2.5);
#514=CIRCLE('',#1445,2.5);
#515=CIRCLE('',#1447,2.5);
#516=CIRCLE('',#1448,2.5);
#517=VERTEX_POINT('',#1871);
#518=VERTEX_POINT('',#1873);
#519=VERTEX_POINT('',#1877);
#520=VERTEX_POINT('',#1878);
#521=VERTEX_POINT('',#1880);
#522=VERTEX_POINT('',#1882);
#523=VERTEX_POINT('',#1886);
#524=VERTEX_POINT('',#1887);
#525=VERTEX_POINT('',#1889);
#526=VERTEX_POINT('',#1891);
#527=VERTEX_POINT('',#1895);
#528=VERTEX_POINT('',#1896);
#529=VERTEX_POINT('',#1898);
#530=VERTEX_POINT('',#1900);
#531=VERTEX_POINT('',#1904);
#532=VERTEX_POINT('',#1905);
#533=VERTEX_POINT('',#1907);
#534=VERTEX_POINT('',#1909);
#535=VERTEX_POINT('',#1913);
#536=VERTEX_POINT('',#1914);
#537=VERTEX_POINT('',#1916);
#538=VERTEX_POINT('',#1918);
#539=VERTEX_POINT('',#1922);
#540=VERTEX_POINT('',#1924);
#541=VERTEX_POINT('',#1928);
#542=VERTEX_POINT('',#1930);
#543=VERTEX_POINT('',#1934);
#544=VERTEX_POINT('',#1936);
#545=VERTEX_POINT('',#1940);
#546=VERTEX_POINT('',#1942);
#547=VERTEX_POINT('',#1946);
#548=VERTEX_POINT('',#1948);
#549=VERTEX_POINT('',#1950);
#550=VERTEX_POINT('',#1953);
#551=VERTEX_POINT('',#1955);
#552=VERTEX_POINT('',#1957);
#553=VERTEX_POINT('',#1960);
#554=VERTEX_POINT('',#1962);
#555=VERTEX_POINT('',#1964);
#556=VERTEX_POINT('',#1967);
#557=VERTEX_POINT('',#1969);
#558=VERTEX_POINT('',#1971);
#559=VERTEX_POINT('',#1974);
#560=VERTEX_POINT('',#1976);
#561=VERTEX_POINT('',#1978);
#562=VERTEX_POINT('',#1980);
#563=VERTEX_POINT('',#1982);
#564=VERTEX_POINT('',#1984);
#565=VERTEX_POINT('',#1986);
#566=VERTEX_POINT('',#1988);
#567=VERTEX_POINT('',#1990);
#568=VERTEX_POINT('',#1992);
#569=VERTEX_POINT('',#1996);
#570=VERTEX_POINT('',#2000);
#571=VERTEX_POINT('',#2002);
#572=VERTEX_POINT('',#2006);
#573=VERTEX_POINT('',#2008);
#574=VERTEX_POINT('',#2010);
#575=VERTEX_POINT('',#2012);
#576=VERTEX_POINT('',#2015);
#577=VERTEX_POINT('',#2017);
#578=VERTEX_POINT('',#2019);
#579=VERTEX_POINT('',#2022);
#580=VERTEX_POINT('',#2024);
#581=VERTEX_POINT('',#2026);
#582=VERTEX_POINT('',#2029);
#583=VERTEX_POINT('',#2031);
#584=VERTEX_POINT('',#2033);
#585=VERTEX_POINT('',#2036);
#586=VERTEX_POINT('',#2038);
#587=VERTEX_POINT('',#2040);
#588=VERTEX_POINT('',#2043);
#589=VERTEX_POINT('',#2045);
#590=VERTEX_POINT('',#2047);
#591=VERTEX_POINT('',#2096);
#592=VERTEX_POINT('',#2099);
#593=VERTEX_POINT('',#2105);
#594=VERTEX_POINT('',#2108);
#595=VERTEX_POINT('',#2114);
#596=VERTEX_POINT('',#2116);
#597=VERTEX_POINT('',#2120);
#598=VERTEX_POINT('',#2123);
#599=VERTEX_POINT('',#2129);
#600=VERTEX_POINT('',#2131);
#601=VERTEX_POINT('',#2134);
#602=VERTEX_POINT('',#2138);
#603=VERTEX_POINT('',#2144);
#604=VERTEX_POINT('',#2146);
#605=VERTEX_POINT('',#2150);
#606=VERTEX_POINT('',#2152);
#607=VERTEX_POINT('',#2156);
#608=VERTEX_POINT('',#2158);
#609=VERTEX_POINT('',#2165);
#610=VERTEX_POINT('',#2168);
#611=VERTEX_POINT('',#2174);
#612=VERTEX_POINT('',#2176);
#613=VERTEX_POINT('',#2180);
#614=VERTEX_POINT('',#2182);
#615=VERTEX_POINT('',#2186);
#616=VERTEX_POINT('',#2187);
#617=VERTEX_POINT('',#2189);
#618=VERTEX_POINT('',#2191);
#619=VERTEX_POINT('',#2195);
#620=VERTEX_POINT('',#2197);
#621=VERTEX_POINT('',#2201);
#622=VERTEX_POINT('',#2205);
#623=EDGE_CURVE('',#517,#517,#443,.T.);
#624=EDGE_CURVE('',#517,#518,#273,.T.);
#625=EDGE_CURVE('',#518,#518,#444,.T.);
#626=EDGE_CURVE('',#519,#520,#274,.T.);
#627=EDGE_CURVE('',#521,#519,#445,.T.);
#628=EDGE_CURVE('',#522,#521,#275,.T.);
#629=EDGE_CURVE('',#520,#522,#446,.T.);
#630=EDGE_CURVE('',#523,#524,#276,.T.);
#631=EDGE_CURVE('',#525,#523,#447,.T.);
#632=EDGE_CURVE('',#526,#525,#277,.T.);
#633=EDGE_CURVE('',#524,#526,#448,.T.);
#634=EDGE_CURVE('',#527,#528,#278,.T.);
#635=EDGE_CURVE('',#529,#527,#449,.T.);
#636=EDGE_CURVE('',#530,#529,#279,.T.);
#637=EDGE_CURVE('',#528,#530,#450,.T.);
#638=EDGE_CURVE('',#531,#532,#280,.T.);
#639=EDGE_CURVE('',#533,#531,#451,.T.);
#640=EDGE_CURVE('',#534,#533,#281,.T.);
#641=EDGE_CURVE('',#532,#534,#452,.T.);
#642=EDGE_CURVE('',#535,#536,#282,.T.);
#643=EDGE_CURVE('',#537,#535,#453,.T.);
#644=EDGE_CURVE('',#538,#537,#283,.T.);
#645=EDGE_CURVE('',#536,#538,#454,.T.);
#646=EDGE_CURVE('',#539,#521,#455,.T.);
#647=EDGE_CURVE('',#540,#539,#284,.T.);
#648=EDGE_CURVE('',#522,#540,#456,.T.);
#649=EDGE_CURVE('',#525,#541,#457,.T.);
#650=EDGE_CURVE('',#542,#541,#285,.T.);
#651=EDGE_CURVE('',#542,#526,#458,.T.);
#652=EDGE_CURVE('',#543,#529,#459,.T.);
#653=EDGE_CURVE('',#544,#543,#286,.T.);
#654=EDGE_CURVE('',#530,#544,#460,.T.);
#655=EDGE_CURVE('',#545,#533,#461,.T.);
#656=EDGE_CURVE('',#546,#545,#287,.T.);
#657=EDGE_CURVE('',#534,#546,#462,.T.);
#658=EDGE_CURVE('',#547,#540,#288,.T.);
#659=EDGE_CURVE('',#547,#548,#463,.T.);
#660=EDGE_CURVE('',#548,#549,#289,.T.);
#661=EDGE_CURVE('',#524,#549,#464,.T.);
#662=EDGE_CURVE('',#542,#550,#290,.T.);
#663=EDGE_CURVE('',#550,#551,#465,.T.);
#664=EDGE_CURVE('',#551,#552,#291,.T.);
#665=EDGE_CURVE('',#552,#528,#466,.T.);
#666=EDGE_CURVE('',#553,#544,#292,.T.);
#667=EDGE_CURVE('',#554,#553,#467,.T.);
#668=EDGE_CURVE('',#555,#554,#293,.T.);
#669=EDGE_CURVE('',#555,#532,#468,.T.);
#670=EDGE_CURVE('',#556,#546,#294,.T.);
#671=EDGE_CURVE('',#557,#556,#469,.T.);
#672=EDGE_CURVE('',#557,#558,#295,.T.);
#673=EDGE_CURVE('',#536,#558,#470,.T.);
#674=EDGE_CURVE('',#559,#538,#471,.T.);
#675=EDGE_CURVE('',#559,#560,#296,.T.);
#676=EDGE_CURVE('',#560,#561,#472,.T.);
#677=EDGE_CURVE('',#561,#562,#297,.T.);
#678=EDGE_CURVE('',#563,#562,#473,.T.);
#679=EDGE_CURVE('',#563,#564,#474,.T.);
#680=EDGE_CURVE('',#565,#564,#475,.T.);
#681=EDGE_CURVE('',#566,#565,#298,.T.);
#682=EDGE_CURVE('',#567,#566,#476,.T.);
#683=EDGE_CURVE('',#568,#567,#299,.T.);
#684=EDGE_CURVE('',#568,#520,#477,.T.);
#685=EDGE_CURVE('',#537,#569,#478,.T.);
#686=EDGE_CURVE('',#559,#569,#300,.T.);
#687=EDGE_CURVE('',#564,#570,#301,.T.);
#688=EDGE_CURVE('',#571,#563,#302,.T.);
#689=EDGE_CURVE('',#570,#571,#479,.T.);
#690=EDGE_CURVE('',#519,#572,#480,.T.);
#691=EDGE_CURVE('',#572,#573,#303,.T.);
#692=EDGE_CURVE('',#573,#574,#481,.T.);
#693=EDGE_CURVE('',#574,#575,#304,.T.);
#694=EDGE_CURVE('',#570,#575,#482,.T.);
#695=EDGE_CURVE('',#576,#571,#483,.T.);
#696=EDGE_CURVE('',#577,#576,#305,.T.);
#697=EDGE_CURVE('',#578,#577,#484,.T.);
#698=EDGE_CURVE('',#569,#578,#306,.T.);
#699=EDGE_CURVE('',#579,#535,#485,.T.);
#700=EDGE_CURVE('',#580,#579,#307,.T.);
#701=EDGE_CURVE('',#581,#580,#486,.T.);
#702=EDGE_CURVE('',#581,#545,#308,.T.);
#703=EDGE_CURVE('',#531,#582,#487,.T.);
#704=EDGE_CURVE('',#582,#583,#309,.T.);
#705=EDGE_CURVE('',#583,#584,#488,.T.);
#706=EDGE_CURVE('',#584,#543,#310,.T.);
#707=EDGE_CURVE('',#527,#585,#489,.T.);
#708=EDGE_CURVE('',#586,#585,#311,.T.);
#709=EDGE_CURVE('',#587,#586,#490,.T.);
#710=EDGE_CURVE('',#541,#587,#312,.T.);
#711=EDGE_CURVE('',#588,#523,#491,.T.);
#712=EDGE_CURVE('',#589,#588,#313,.T.);
#713=EDGE_CURVE('',#589,#590,#492,.T.);
#714=EDGE_CURVE('',#590,#539,#314,.T.);
#715=EDGE_CURVE('',#562,#576,#315,.T.);
#716=EDGE_CURVE('',#565,#575,#316,.T.);
#717=EDGE_CURVE('',#566,#574,#317,.T.);
#718=EDGE_CURVE('',#567,#573,#318,.T.);
#719=EDGE_CURVE('',#568,#572,#319,.T.);
#720=EDGE_CURVE('',#547,#590,#320,.T.);
#721=EDGE_CURVE('',#561,#577,#321,.T.);
#722=EDGE_CURVE('',#560,#578,#322,.T.);
#723=EDGE_CURVE('',#558,#579,#323,.T.);
#724=EDGE_CURVE('',#557,#580,#324,.T.);
#725=EDGE_CURVE('',#551,#586,#325,.T.);
#726=EDGE_CURVE('',#552,#585,#326,.T.);
#727=EDGE_CURVE('',#550,#587,#327,.T.);
#728=EDGE_CURVE('',#549,#588,#328,.T.);
#729=EDGE_CURVE('',#548,#589,#329,.T.);
#730=EDGE_CURVE('',#553,#584,#330,.T.);
#731=EDGE_CURVE('',#554,#583,#331,.T.);
#732=EDGE_CURVE('',#555,#582,#332,.T.);
#733=EDGE_CURVE('',#556,#581,#333,.T.);
#734=EDGE_CURVE('',#591,#591,#493,.T.);
#735=EDGE_CURVE('',#591,#592,#334,.T.);
#736=EDGE_CURVE('',#592,#592,#494,.T.);
#737=EDGE_CURVE('',#593,#593,#495,.T.);
#738=EDGE_CURVE('',#593,#594,#335,.T.);
#739=EDGE_CURVE('',#594,#594,#496,.T.);
#740=EDGE_CURVE('',#595,#595,#497,.T.);
#741=EDGE_CURVE('',#595,#596,#336,.T.);
#742=EDGE_CURVE('',#596,#596,#498,.T.);
#743=EDGE_CURVE('',#597,#597,#499,.T.);
#744=EDGE_CURVE('',#597,#598,#337,.T.);
#745=EDGE_CURVE('',#598,#598,#500,.T.);
#746=EDGE_CURVE('',#599,#599,#501,.T.);
#747=EDGE_CURVE('',#600,#600,#502,.T.);
#748=EDGE_CURVE('',#599,#601,#338,.T.);
#749=EDGE_CURVE('',#601,#601,#503,.T.);
#750=EDGE_CURVE('',#602,#602,#504,.T.);
#751=EDGE_CURVE('',#602,#600,#339,.T.);
#752=EDGE_CURVE('',#603,#603,#505,.T.);
#753=EDGE_CURVE('',#603,#604,#340,.T.);
#754=EDGE_CURVE('',#604,#604,#506,.T.);
#755=EDGE_CURVE('',#605,#605,#507,.T.);
#756=EDGE_CURVE('',#605,#606,#341,.T.);
#757=EDGE_CURVE('',#606,#606,#508,.T.);
#758=EDGE_CURVE('',#607,#607,#509,.T.);
#759=EDGE_CURVE('',#607,#608,#342,.T.);
#760=EDGE_CURVE('',#608,#608,#510,.T.);
#761=EDGE_CURVE('',#609,#609,#511,.T.);
#762=EDGE_CURVE('',#609,#610,#343,.T.);
#763=EDGE_CURVE('',#610,#610,#512,.T.);
#764=EDGE_CURVE('',#611,#611,#513,.T.);
#765=EDGE_CURVE('',#611,#612,#344,.T.);
#766=EDGE_CURVE('',#612,#612,#514,.T.);
#767=EDGE_CURVE('',#613,#613,#515,.T.);
#768=EDGE_CURVE('',#613,#614,#345,.T.);
#769=EDGE_CURVE('',#614,#614,#516,.T.);
#770=EDGE_CURVE('',#615,#616,#346,.T.);
#771=EDGE_CURVE('',#617,#615,#347,.T.);
#772=EDGE_CURVE('',#618,#617,#348,.T.);
#773=EDGE_CURVE('',#616,#618,#349,.T.);
#774=EDGE_CURVE('',#615,#619,#350,.T.);
#775=EDGE_CURVE('',#620,#619,#351,.T.);
#776=EDGE_CURVE('',#617,#620,#352,.T.);
#777=EDGE_CURVE('',#616,#621,#353,.T.);
#778=EDGE_CURVE('',#619,#621,#354,.T.);
#779=EDGE_CURVE('',#622,#620,#355,.T.);
#780=EDGE_CURVE('',#618,#622,#356,.T.);
#781=EDGE_CURVE('',#621,#622,#357,.T.);
#782=ORIENTED_EDGE('',*,*,#623,.F.);
#783=ORIENTED_EDGE('',*,*,#624,.T.);
#784=ORIENTED_EDGE('',*,*,#625,.F.);
#785=ORIENTED_EDGE('',*,*,#624,.F.);
#786=ORIENTED_EDGE('',*,*,#626,.F.);
#787=ORIENTED_EDGE('',*,*,#627,.F.);
#788=ORIENTED_EDGE('',*,*,#628,.F.);
#789=ORIENTED_EDGE('',*,*,#629,.F.);
#790=ORIENTED_EDGE('',*,*,#630,.F.);
#791=ORIENTED_EDGE('',*,*,#631,.F.);
#792=ORIENTED_EDGE('',*,*,#632,.F.);
#793=ORIENTED_EDGE('',*,*,#633,.F.);
#794=ORIENTED_EDGE('',*,*,#634,.F.);
#795=ORIENTED_EDGE('',*,*,#635,.F.);
#796=ORIENTED_EDGE('',*,*,#636,.F.);
#797=ORIENTED_EDGE('',*,*,#637,.F.);
#798=ORIENTED_EDGE('',*,*,#638,.F.);
#799=ORIENTED_EDGE('',*,*,#639,.F.);
#800=ORIENTED_EDGE('',*,*,#640,.F.);
#801=ORIENTED_EDGE('',*,*,#641,.F.);
#802=ORIENTED_EDGE('',*,*,#642,.F.);
#803=ORIENTED_EDGE('',*,*,#643,.F.);
#804=ORIENTED_EDGE('',*,*,#644,.F.);
#805=ORIENTED_EDGE('',*,*,#645,.F.);
#806=ORIENTED_EDGE('',*,*,#628,.T.);
#807=ORIENTED_EDGE('',*,*,#646,.F.);
#808=ORIENTED_EDGE('',*,*,#647,.F.);
#809=ORIENTED_EDGE('',*,*,#648,.F.);
#810=ORIENTED_EDGE('',*,*,#632,.T.);
#811=ORIENTED_EDGE('',*,*,#649,.T.);
#812=ORIENTED_EDGE('',*,*,#650,.F.);
#813=ORIENTED_EDGE('',*,*,#651,.T.);
#814=ORIENTED_EDGE('',*,*,#636,.T.);
#815=ORIENTED_EDGE('',*,*,#652,.F.);
#816=ORIENTED_EDGE('',*,*,#653,.F.);
#817=ORIENTED_EDGE('',*,*,#654,.F.);
#818=ORIENTED_EDGE('',*,*,#640,.T.);
#819=ORIENTED_EDGE('',*,*,#655,.F.);
#820=ORIENTED_EDGE('',*,*,#656,.F.);
#821=ORIENTED_EDGE('',*,*,#657,.F.);
#822=ORIENTED_EDGE('',*,*,#629,.T.);
#823=ORIENTED_EDGE('',*,*,#648,.T.);
#824=ORIENTED_EDGE('',*,*,#658,.F.);
#825=ORIENTED_EDGE('',*,*,#659,.T.);
#826=ORIENTED_EDGE('',*,*,#660,.T.);
#827=ORIENTED_EDGE('',*,*,#661,.F.);
#828=ORIENTED_EDGE('',*,*,#633,.T.);
#829=ORIENTED_EDGE('',*,*,#651,.F.);
#830=ORIENTED_EDGE('',*,*,#662,.T.);
#831=ORIENTED_EDGE('',*,*,#663,.T.);
#832=ORIENTED_EDGE('',*,*,#664,.T.);
#833=ORIENTED_EDGE('',*,*,#665,.T.);
#834=ORIENTED_EDGE('',*,*,#637,.T.);
#835=ORIENTED_EDGE('',*,*,#654,.T.);
#836=ORIENTED_EDGE('',*,*,#666,.F.);
#837=ORIENTED_EDGE('',*,*,#667,.F.);
#838=ORIENTED_EDGE('',*,*,#668,.F.);
#839=ORIENTED_EDGE('',*,*,#669,.T.);
#840=ORIENTED_EDGE('',*,*,#641,.T.);
#841=ORIENTED_EDGE('',*,*,#657,.T.);
#842=ORIENTED_EDGE('',*,*,#670,.F.);
#843=ORIENTED_EDGE('',*,*,#671,.F.);
#844=ORIENTED_EDGE('',*,*,#672,.T.);
#845=ORIENTED_EDGE('',*,*,#673,.F.);
#846=ORIENTED_EDGE('',*,*,#645,.T.);
#847=ORIENTED_EDGE('',*,*,#674,.F.);
#848=ORIENTED_EDGE('',*,*,#675,.T.);
#849=ORIENTED_EDGE('',*,*,#676,.T.);
#850=ORIENTED_EDGE('',*,*,#677,.T.);
#851=ORIENTED_EDGE('',*,*,#678,.F.);
#852=ORIENTED_EDGE('',*,*,#679,.T.);
#853=ORIENTED_EDGE('',*,*,#680,.F.);
#854=ORIENTED_EDGE('',*,*,#681,.F.);
#855=ORIENTED_EDGE('',*,*,#682,.F.);
#856=ORIENTED_EDGE('',*,*,#683,.F.);
#857=ORIENTED_EDGE('',*,*,#684,.T.);
#858=ORIENTED_EDGE('',*,*,#623,.T.);
#859=ORIENTED_EDGE('',*,*,#644,.T.);
#860=ORIENTED_EDGE('',*,*,#685,.T.);
#861=ORIENTED_EDGE('',*,*,#686,.F.);
#862=ORIENTED_EDGE('',*,*,#674,.T.);
#863=ORIENTED_EDGE('',*,*,#687,.F.);
#864=ORIENTED_EDGE('',*,*,#679,.F.);
#865=ORIENTED_EDGE('',*,*,#688,.F.);
#866=ORIENTED_EDGE('',*,*,#689,.F.);
#867=ORIENTED_EDGE('',*,*,#627,.T.);
#868=ORIENTED_EDGE('',*,*,#690,.T.);
#869=ORIENTED_EDGE('',*,*,#691,.T.);
#870=ORIENTED_EDGE('',*,*,#692,.T.);
#871=ORIENTED_EDGE('',*,*,#693,.T.);
#872=ORIENTED_EDGE('',*,*,#694,.F.);
#873=ORIENTED_EDGE('',*,*,#689,.T.);
#874=ORIENTED_EDGE('',*,*,#695,.F.);
#875=ORIENTED_EDGE('',*,*,#696,.F.);
#876=ORIENTED_EDGE('',*,*,#697,.F.);
#877=ORIENTED_EDGE('',*,*,#698,.F.);
#878=ORIENTED_EDGE('',*,*,#685,.F.);
#879=ORIENTED_EDGE('',*,*,#643,.T.);
#880=ORIENTED_EDGE('',*,*,#699,.F.);
#881=ORIENTED_EDGE('',*,*,#700,.F.);
#882=ORIENTED_EDGE('',*,*,#701,.F.);
#883=ORIENTED_EDGE('',*,*,#702,.T.);
#884=ORIENTED_EDGE('',*,*,#655,.T.);
#885=ORIENTED_EDGE('',*,*,#639,.T.);
#886=ORIENTED_EDGE('',*,*,#703,.T.);
#887=ORIENTED_EDGE('',*,*,#704,.T.);
#888=ORIENTED_EDGE('',*,*,#705,.T.);
#889=ORIENTED_EDGE('',*,*,#706,.T.);
#890=ORIENTED_EDGE('',*,*,#652,.T.);
#891=ORIENTED_EDGE('',*,*,#635,.T.);
#892=ORIENTED_EDGE('',*,*,#707,.T.);
#893=ORIENTED_EDGE('',*,*,#708,.F.);
#894=ORIENTED_EDGE('',*,*,#709,.F.);
#895=ORIENTED_EDGE('',*,*,#710,.F.);
#896=ORIENTED_EDGE('',*,*,#649,.F.);
#897=ORIENTED_EDGE('',*,*,#631,.T.);
#898=ORIENTED_EDGE('',*,*,#711,.F.);
#899=ORIENTED_EDGE('',*,*,#712,.F.);
#900=ORIENTED_EDGE('',*,*,#713,.T.);
#901=ORIENTED_EDGE('',*,*,#714,.T.);
#902=ORIENTED_EDGE('',*,*,#646,.T.);
#903=ORIENTED_EDGE('',*,*,#625,.T.);
#904=ORIENTED_EDGE('',*,*,#688,.T.);
#905=ORIENTED_EDGE('',*,*,#678,.T.);
#906=ORIENTED_EDGE('',*,*,#715,.T.);
#907=ORIENTED_EDGE('',*,*,#695,.T.);
#908=ORIENTED_EDGE('',*,*,#687,.T.);
#909=ORIENTED_EDGE('',*,*,#694,.T.);
#910=ORIENTED_EDGE('',*,*,#716,.F.);
#911=ORIENTED_EDGE('',*,*,#680,.T.);
#912=ORIENTED_EDGE('',*,*,#681,.T.);
#913=ORIENTED_EDGE('',*,*,#716,.T.);
#914=ORIENTED_EDGE('',*,*,#693,.F.);
#915=ORIENTED_EDGE('',*,*,#717,.F.);
#916=ORIENTED_EDGE('',*,*,#682,.T.);
#917=ORIENTED_EDGE('',*,*,#717,.T.);
#918=ORIENTED_EDGE('',*,*,#692,.F.);
#919=ORIENTED_EDGE('',*,*,#718,.F.);
#920=ORIENTED_EDGE('',*,*,#683,.T.);
#921=ORIENTED_EDGE('',*,*,#718,.T.);
#922=ORIENTED_EDGE('',*,*,#691,.F.);
#923=ORIENTED_EDGE('',*,*,#719,.F.);
#924=ORIENTED_EDGE('',*,*,#626,.T.);
#925=ORIENTED_EDGE('',*,*,#684,.F.);
#926=ORIENTED_EDGE('',*,*,#719,.T.);
#927=ORIENTED_EDGE('',*,*,#690,.F.);
#928=ORIENTED_EDGE('',*,*,#658,.T.);
#929=ORIENTED_EDGE('',*,*,#647,.T.);
#930=ORIENTED_EDGE('',*,*,#714,.F.);
#931=ORIENTED_EDGE('',*,*,#720,.F.);
#932=ORIENTED_EDGE('',*,*,#677,.F.);
#933=ORIENTED_EDGE('',*,*,#721,.T.);
#934=ORIENTED_EDGE('',*,*,#696,.T.);
#935=ORIENTED_EDGE('',*,*,#715,.F.);
#936=ORIENTED_EDGE('',*,*,#676,.F.);
#937=ORIENTED_EDGE('',*,*,#722,.T.);
#938=ORIENTED_EDGE('',*,*,#697,.T.);
#939=ORIENTED_EDGE('',*,*,#721,.F.);
#940=ORIENTED_EDGE('',*,*,#675,.F.);
#941=ORIENTED_EDGE('',*,*,#686,.T.);
#942=ORIENTED_EDGE('',*,*,#698,.T.);
#943=ORIENTED_EDGE('',*,*,#722,.F.);
#944=ORIENTED_EDGE('',*,*,#642,.T.);
#945=ORIENTED_EDGE('',*,*,#673,.T.);
#946=ORIENTED_EDGE('',*,*,#723,.T.);
#947=ORIENTED_EDGE('',*,*,#699,.T.);
#948=ORIENTED_EDGE('',*,*,#672,.F.);
#949=ORIENTED_EDGE('',*,*,#724,.T.);
#950=ORIENTED_EDGE('',*,*,#700,.T.);
#951=ORIENTED_EDGE('',*,*,#723,.F.);
#952=ORIENTED_EDGE('',*,*,#664,.F.);
#953=ORIENTED_EDGE('',*,*,#725,.T.);
#954=ORIENTED_EDGE('',*,*,#708,.T.);
#955=ORIENTED_EDGE('',*,*,#726,.F.);
#956=ORIENTED_EDGE('',*,*,#663,.F.);
#957=ORIENTED_EDGE('',*,*,#727,.T.);
#958=ORIENTED_EDGE('',*,*,#709,.T.);
#959=ORIENTED_EDGE('',*,*,#725,.F.);
#960=ORIENTED_EDGE('',*,*,#662,.F.);
#961=ORIENTED_EDGE('',*,*,#650,.T.);
#962=ORIENTED_EDGE('',*,*,#710,.T.);
#963=ORIENTED_EDGE('',*,*,#727,.F.);
#964=ORIENTED_EDGE('',*,*,#630,.T.);
#965=ORIENTED_EDGE('',*,*,#661,.T.);
#966=ORIENTED_EDGE('',*,*,#728,.T.);
#967=ORIENTED_EDGE('',*,*,#711,.T.);
#968=ORIENTED_EDGE('',*,*,#660,.F.);
#969=ORIENTED_EDGE('',*,*,#729,.T.);
#970=ORIENTED_EDGE('',*,*,#712,.T.);
#971=ORIENTED_EDGE('',*,*,#728,.F.);
#972=ORIENTED_EDGE('',*,*,#659,.F.);
#973=ORIENTED_EDGE('',*,*,#720,.T.);
#974=ORIENTED_EDGE('',*,*,#713,.F.);
#975=ORIENTED_EDGE('',*,*,#729,.F.);
#976=ORIENTED_EDGE('',*,*,#634,.T.);
#977=ORIENTED_EDGE('',*,*,#665,.F.);
#978=ORIENTED_EDGE('',*,*,#726,.T.);
#979=ORIENTED_EDGE('',*,*,#707,.F.);
#980=ORIENTED_EDGE('',*,*,#666,.T.);
#981=ORIENTED_EDGE('',*,*,#653,.T.);
#982=ORIENTED_EDGE('',*,*,#706,.F.);
#983=ORIENTED_EDGE('',*,*,#730,.F.);
#984=ORIENTED_EDGE('',*,*,#667,.T.);
#985=ORIENTED_EDGE('',*,*,#730,.T.);
#986=ORIENTED_EDGE('',*,*,#705,.F.);
#987=ORIENTED_EDGE('',*,*,#731,.F.);
#988=ORIENTED_EDGE('',*,*,#668,.T.);
#989=ORIENTED_EDGE('',*,*,#731,.T.);
#990=ORIENTED_EDGE('',*,*,#704,.F.);
#991=ORIENTED_EDGE('',*,*,#732,.F.);
#992=ORIENTED_EDGE('',*,*,#638,.T.);
#993=ORIENTED_EDGE('',*,*,#669,.F.);
#994=ORIENTED_EDGE('',*,*,#732,.T.);
#995=ORIENTED_EDGE('',*,*,#703,.F.);
#996=ORIENTED_EDGE('',*,*,#670,.T.);
#997=ORIENTED_EDGE('',*,*,#656,.T.);
#998=ORIENTED_EDGE('',*,*,#702,.F.);
#999=ORIENTED_EDGE('',*,*,#733,.F.);
#1000=ORIENTED_EDGE('',*,*,#671,.T.);
#1001=ORIENTED_EDGE('',*,*,#733,.T.);
#1002=ORIENTED_EDGE('',*,*,#701,.T.);
#1003=ORIENTED_EDGE('',*,*,#724,.F.);
#1004=ORIENTED_EDGE('',*,*,#734,.T.);
#1005=ORIENTED_EDGE('',*,*,#734,.F.);
#1006=ORIENTED_EDGE('',*,*,#735,.T.);
#1007=ORIENTED_EDGE('',*,*,#736,.T.);
#1008=ORIENTED_EDGE('',*,*,#735,.F.);
#1009=ORIENTED_EDGE('',*,*,#736,.F.);
#1010=ORIENTED_EDGE('',*,*,#737,.T.);
#1011=ORIENTED_EDGE('',*,*,#737,.F.);
#1012=ORIENTED_EDGE('',*,*,#738,.T.);
#1013=ORIENTED_EDGE('',*,*,#739,.T.);
#1014=ORIENTED_EDGE('',*,*,#738,.F.);
#1015=ORIENTED_EDGE('',*,*,#739,.F.);
#1016=ORIENTED_EDGE('',*,*,#740,.F.);
#1017=ORIENTED_EDGE('',*,*,#741,.T.);
#1018=ORIENTED_EDGE('',*,*,#742,.F.);
#1019=ORIENTED_EDGE('',*,*,#741,.F.);
#1020=ORIENTED_EDGE('',*,*,#743,.T.);
#1021=ORIENTED_EDGE('',*,*,#742,.T.);
#1022=ORIENTED_EDGE('',*,*,#743,.F.);
#1023=ORIENTED_EDGE('',*,*,#744,.T.);
#1024=ORIENTED_EDGE('',*,*,#745,.T.);
#1025=ORIENTED_EDGE('',*,*,#744,.F.);
#1026=ORIENTED_EDGE('',*,*,#745,.F.);
#1027=ORIENTED_EDGE('',*,*,#740,.T.);
#1028=ORIENTED_EDGE('',*,*,#746,.T.);
#1029=ORIENTED_EDGE('',*,*,#747,.F.);
#1030=ORIENTED_EDGE('',*,*,#746,.F.);
#1031=ORIENTED_EDGE('',*,*,#748,.T.);
#1032=ORIENTED_EDGE('',*,*,#749,.F.);
#1033=ORIENTED_EDGE('',*,*,#748,.F.);
#1034=ORIENTED_EDGE('',*,*,#750,.F.);
#1035=ORIENTED_EDGE('',*,*,#751,.T.);
#1036=ORIENTED_EDGE('',*,*,#747,.T.);
#1037=ORIENTED_EDGE('',*,*,#751,.F.);
#1038=ORIENTED_EDGE('',*,*,#749,.T.);
#1039=ORIENTED_EDGE('',*,*,#750,.T.);
#1040=ORIENTED_EDGE('',*,*,#752,.F.);
#1041=ORIENTED_EDGE('',*,*,#753,.T.);
#1042=ORIENTED_EDGE('',*,*,#754,.F.);
#1043=ORIENTED_EDGE('',*,*,#753,.F.);
#1044=ORIENTED_EDGE('',*,*,#755,.F.);
#1045=ORIENTED_EDGE('',*,*,#756,.T.);
#1046=ORIENTED_EDGE('',*,*,#757,.F.);
#1047=ORIENTED_EDGE('',*,*,#756,.F.);
#1048=ORIENTED_EDGE('',*,*,#758,.F.);
#1049=ORIENTED_EDGE('',*,*,#759,.T.);
#1050=ORIENTED_EDGE('',*,*,#760,.T.);
#1051=ORIENTED_EDGE('',*,*,#759,.F.);
#1052=ORIENTED_EDGE('',*,*,#758,.T.);
#1053=ORIENTED_EDGE('',*,*,#752,.T.);
#1054=ORIENTED_EDGE('',*,*,#755,.T.);
#1055=ORIENTED_EDGE('',*,*,#760,.F.);
#1056=ORIENTED_EDGE('',*,*,#754,.T.);
#1057=ORIENTED_EDGE('',*,*,#757,.T.);
#1058=ORIENTED_EDGE('',*,*,#761,.T.);
#1059=ORIENTED_EDGE('',*,*,#761,.F.);
#1060=ORIENTED_EDGE('',*,*,#762,.T.);
#1061=ORIENTED_EDGE('',*,*,#763,.T.);
#1062=ORIENTED_EDGE('',*,*,#762,.F.);
#1063=ORIENTED_EDGE('',*,*,#763,.F.);
#1064=ORIENTED_EDGE('',*,*,#764,.F.);
#1065=ORIENTED_EDGE('',*,*,#765,.T.);
#1066=ORIENTED_EDGE('',*,*,#766,.F.);
#1067=ORIENTED_EDGE('',*,*,#765,.F.);
#1068=ORIENTED_EDGE('',*,*,#767,.F.);
#1069=ORIENTED_EDGE('',*,*,#768,.T.);
#1070=ORIENTED_EDGE('',*,*,#769,.T.);
#1071=ORIENTED_EDGE('',*,*,#768,.F.);
#1072=ORIENTED_EDGE('',*,*,#770,.F.);
#1073=ORIENTED_EDGE('',*,*,#771,.F.);
#1074=ORIENTED_EDGE('',*,*,#772,.F.);
#1075=ORIENTED_EDGE('',*,*,#773,.F.);
#1076=ORIENTED_EDGE('',*,*,#769,.F.);
#1077=ORIENTED_EDGE('',*,*,#766,.T.);
#1078=ORIENTED_EDGE('',*,*,#771,.T.);
#1079=ORIENTED_EDGE('',*,*,#774,.T.);
#1080=ORIENTED_EDGE('',*,*,#775,.F.);
#1081=ORIENTED_EDGE('',*,*,#776,.F.);
#1082=ORIENTED_EDGE('',*,*,#770,.T.);
#1083=ORIENTED_EDGE('',*,*,#777,.T.);
#1084=ORIENTED_EDGE('',*,*,#778,.F.);
#1085=ORIENTED_EDGE('',*,*,#774,.F.);
#1086=ORIENTED_EDGE('',*,*,#772,.T.);
#1087=ORIENTED_EDGE('',*,*,#776,.T.);
#1088=ORIENTED_EDGE('',*,*,#779,.F.);
#1089=ORIENTED_EDGE('',*,*,#780,.F.);
#1090=ORIENTED_EDGE('',*,*,#773,.T.);
#1091=ORIENTED_EDGE('',*,*,#780,.T.);
#1092=ORIENTED_EDGE('',*,*,#781,.F.);
#1093=ORIENTED_EDGE('',*,*,#777,.F.);
#1094=ORIENTED_EDGE('',*,*,#778,.T.);
#1095=ORIENTED_EDGE('',*,*,#781,.T.);
#1096=ORIENTED_EDGE('',*,*,#779,.T.);
#1097=ORIENTED_EDGE('',*,*,#775,.T.);
#1098=ORIENTED_EDGE('',*,*,#764,.T.);
#1099=ORIENTED_EDGE('',*,*,#767,.T.);
#1100=CYLINDRICAL_SURFACE('',#1305,2.5);
#1101=CYLINDRICAL_SURFACE('',#1308,13.);
#1102=CYLINDRICAL_SURFACE('',#1311,13.);
#1103=CYLINDRICAL_SURFACE('',#1314,13.);
#1104=CYLINDRICAL_SURFACE('',#1317,13.);
#1105=CYLINDRICAL_SURFACE('',#1320,13.);
#1106=CYLINDRICAL_SURFACE('',#1323,35.);
#1107=CYLINDRICAL_SURFACE('',#1326,35.);
#1108=CYLINDRICAL_SURFACE('',#1329,35.);
#1109=CYLINDRICAL_SURFACE('',#1332,35.);
#1110=CYLINDRICAL_SURFACE('',#1351,35.);
#1111=CYLINDRICAL_SURFACE('',#1353,13.);
#1112=CYLINDRICAL_SURFACE('',#1369,35.);
#1113=CYLINDRICAL_SURFACE('',#1370,35.);
#1114=CYLINDRICAL_SURFACE('',#1372,2.5);
#1115=CYLINDRICAL_SURFACE('',#1374,35.);
#1116=CYLINDRICAL_SURFACE('',#1377,2.5);
#1117=CYLINDRICAL_SURFACE('',#1379,35.);
#1118=CYLINDRICAL_SURFACE('',#1382,2.5);
#1119=CYLINDRICAL_SURFACE('',#1384,35.);
#1120=CYLINDRICAL_SURFACE('',#1386,2.5);
#1121=CYLINDRICAL_SURFACE('',#1387,35.);
#1122=CYLINDRICAL_SURFACE('',#1389,2.5);
#1123=CYLINDRICAL_SURFACE('',#1391,35.);
#1124=CYLINDRICAL_SURFACE('',#1393,2.5);
#1125=CYLINDRICAL_SURFACE('',#1397,2.25);
#1126=CYLINDRICAL_SURFACE('',#1403,2.5);
#1127=CYLINDRICAL_SURFACE('',#1407,2.5);
#1128=CYLINDRICAL_SURFACE('',#1412,13.);
#1129=CYLINDRICAL_SURFACE('',#1419,4.5);
#1130=CYLINDRICAL_SURFACE('',#1421,2.5);
#1131=CYLINDRICAL_SURFACE('',#1425,13.);
#1132=CYLINDRICAL_SURFACE('',#1428,2.25);
#1133=CYLINDRICAL_SURFACE('',#1431,24.1717785126239);
#1134=CYLINDRICAL_SURFACE('',#1439,2.5);
#1135=CYLINDRICAL_SURFACE('',#1443,2.5);
#1136=CYLINDRICAL_SURFACE('',#1446,2.5);
#1137=ADVANCED_FACE('',(#121),#1100,.F.);
#1138=ADVANCED_FACE('',(#122),#1101,.F.);
#1139=ADVANCED_FACE('',(#123),#1102,.F.);
#1140=ADVANCED_FACE('',(#124),#1103,.F.);
#1141=ADVANCED_FACE('',(#125),#1104,.F.);
#1142=ADVANCED_FACE('',(#126),#1105,.F.);
#1143=ADVANCED_FACE('',(#127),#1106,.T.);
#1144=ADVANCED_FACE('',(#128),#1107,.T.);
#1145=ADVANCED_FACE('',(#129),#1108,.T.);
#1146=ADVANCED_FACE('',(#130),#1109,.T.);
#1147=ADVANCED_FACE('',(#131,#75),#89,.T.);
#1148=ADVANCED_FACE('',(#132),#1110,.T.);
#1149=ADVANCED_FACE('',(#133),#1111,.F.);
#1150=ADVANCED_FACE('',(#134,#76),#90,.F.);
#1151=ADVANCED_FACE('',(#135),#1112,.T.);
#1152=ADVANCED_FACE('',(#136),#1113,.T.);
#1153=ADVANCED_FACE('',(#137),#91,.T.);
#1154=ADVANCED_FACE('',(#138),#1114,.F.);
#1155=ADVANCED_FACE('',(#139),#92,.T.);
#1156=ADVANCED_FACE('',(#140),#1115,.T.);
#1157=ADVANCED_FACE('',(#141),#93,.T.);
#1158=ADVANCED_FACE('',(#142),#94,.F.);
#1159=ADVANCED_FACE('',(#143),#1116,.F.);
#1160=ADVANCED_FACE('',(#144),#95,.F.);
#1161=ADVANCED_FACE('',(#145),#1117,.T.);
#1162=ADVANCED_FACE('',(#146),#96,.F.);
#1163=ADVANCED_FACE('',(#147),#97,.F.);
#1164=ADVANCED_FACE('',(#148),#1118,.F.);
#1165=ADVANCED_FACE('',(#149),#98,.F.);
#1166=ADVANCED_FACE('',(#150),#1119,.T.);
#1167=ADVANCED_FACE('',(#151),#99,.F.);
#1168=ADVANCED_FACE('',(#152),#1120,.F.);
#1169=ADVANCED_FACE('',(#153),#1121,.T.);
#1170=ADVANCED_FACE('',(#154),#100,.T.);
#1171=ADVANCED_FACE('',(#155),#1122,.F.);
#1172=ADVANCED_FACE('',(#156),#101,.T.);
#1173=ADVANCED_FACE('',(#157),#1123,.T.);
#1174=ADVANCED_FACE('',(#158),#102,.T.);
#1175=ADVANCED_FACE('',(#159),#1124,.F.);
#1176=ADVANCED_FACE('',(#160),#103,.F.);
#1177=ADVANCED_FACE('',(#161),#1125,.T.);
#1178=ADVANCED_FACE('',(#162),#104,.T.);
#1179=ADVANCED_FACE('',(#163),#105,.T.);
#1180=ADVANCED_FACE('',(#164),#1126,.T.);
#1181=ADVANCED_FACE('',(#165),#106,.T.);
#1182=ADVANCED_FACE('',(#166),#1127,.F.);
#1183=ADVANCED_FACE('',(#167,#77),#107,.F.);
#1184=ADVANCED_FACE('',(#168),#1128,.T.);
#1185=ADVANCED_FACE('',(#169,#78),#108,.T.);
#1186=ADVANCED_FACE('',(#170,#79),#109,.T.);
#1187=ADVANCED_FACE('',(#171),#1129,.T.);
#1188=ADVANCED_FACE('',(#172),#1130,.F.);
#1189=ADVANCED_FACE('',(#173,#80),#110,.T.);
#1190=ADVANCED_FACE('',(#174),#1131,.F.);
#1191=ADVANCED_FACE('',(#175),#1132,.F.);
#1192=ADVANCED_FACE('',(#176),#1133,.T.);
#1193=ADVANCED_FACE('',(#177,#81,#82),#111,.T.);
#1194=ADVANCED_FACE('',(#178,#83,#84),#112,.F.);
#1195=ADVANCED_FACE('',(#179),#113,.T.);
#1196=ADVANCED_FACE('',(#180),#1134,.T.);
#1197=ADVANCED_FACE('',(#181),#114,.T.);
#1198=ADVANCED_FACE('',(#182),#1135,.F.);
#1199=ADVANCED_FACE('',(#183),#1136,.F.);
#1200=ADVANCED_FACE('',(#184,#85,#86),#115,.F.);
#1201=ADVANCED_FACE('',(#185),#116,.T.);
#1202=ADVANCED_FACE('',(#186),#117,.T.);
#1203=ADVANCED_FACE('',(#187),#118,.T.);
#1204=ADVANCED_FACE('',(#188),#119,.T.);
#1205=ADVANCED_FACE('',(#189,#87,#88),#120,.T.);
#1206=CLOSED_SHELL('',(#1137,#1138,#1139,#1140,#1141,#1142,#1143,#1144,
#1145,#1146,#1147,#1148,#1149,#1150,#1151,#1152,#1153,#1154,#1155,#1156,
#1157,#1158,#1159,#1160,#1161,#1162,#1163,#1164,#1165,#1166,#1167,#1168,
#1169,#1170,#1171,#1172,#1173,#1174,#1175));
#1207=CLOSED_SHELL('',(#1176,#1177,#1178));
#1208=CLOSED_SHELL('',(#1179,#1180,#1181));
#1209=CLOSED_SHELL('',(#1182,#1183,#1184,#1185));
#1210=CLOSED_SHELL('',(#1186,#1187,#1188,#1189));
#1211=CLOSED_SHELL('',(#1190,#1191,#1192,#1193,#1194));
#1212=CLOSED_SHELL('',(#1195,#1196,#1197));
#1213=CLOSED_SHELL('',(#1198,#1199,#1200,#1201,#1202,#1203,#1204,#1205));
#1214=DERIVED_UNIT_ELEMENT(#1230,1.);
#1215=DERIVED_UNIT_ELEMENT(#2240,-3.);
#1216=DERIVED_UNIT_ELEMENT(#1230,1.);
#1217=DERIVED_UNIT_ELEMENT(#2240,-3.);
#1218=DERIVED_UNIT_ELEMENT(#1230,1.);
#1219=DERIVED_UNIT_ELEMENT(#2240,-3.);
#1220=DERIVED_UNIT_ELEMENT(#1230,1.);
#1221=DERIVED_UNIT_ELEMENT(#2240,-3.);
#1222=DERIVED_UNIT_ELEMENT(#1230,1.);
#1223=DERIVED_UNIT_ELEMENT(#2240,-3.);
#1224=DERIVED_UNIT_ELEMENT(#1230,1.);
#1225=DERIVED_UNIT_ELEMENT(#2240,-3.);
#1226=DERIVED_UNIT_ELEMENT(#1230,1.);
#1227=DERIVED_UNIT_ELEMENT(#2240,-3.);
#1228=DERIVED_UNIT_ELEMENT(#1230,1.);
#1229=DERIVED_UNIT_ELEMENT(#2240,-3.);
#1230=(
MASS_UNIT()
NAMED_UNIT(*)
SI_UNIT(.KILO.,.GRAM.)
);
#1231=DERIVED_UNIT((#1214,#1215));
#1232=DERIVED_UNIT((#1216,#1217));
#1233=DERIVED_UNIT((#1218,#1219));
#1234=DERIVED_UNIT((#1220,#1221));
#1235=DERIVED_UNIT((#1222,#1223));
#1236=DERIVED_UNIT((#1224,#1225));
#1237=DERIVED_UNIT((#1226,#1227));
#1238=DERIVED_UNIT((#1228,#1229));
#1239=MEASURE_REPRESENTATION_ITEM('density measure',
POSITIVE_RATIO_MEASURE(7850.),#1231);
#1240=MEASURE_REPRESENTATION_ITEM('density measure',
POSITIVE_RATIO_MEASURE(7850.),#1232);
#1241=MEASURE_REPRESENTATION_ITEM('density measure',
POSITIVE_RATIO_MEASURE(7850.),#1233);
#1242=MEASURE_REPRESENTATION_ITEM('density measure',
POSITIVE_RATIO_MEASURE(7850.),#1234);
#1243=MEASURE_REPRESENTATION_ITEM('density measure',
POSITIVE_RATIO_MEASURE(7850.),#1235);
#1244=MEASURE_REPRESENTATION_ITEM('density measure',
POSITIVE_RATIO_MEASURE(7850.),#1236);
#1245=MEASURE_REPRESENTATION_ITEM('density measure',
POSITIVE_RATIO_MEASURE(7850.),#1237);
#1246=MEASURE_REPRESENTATION_ITEM('density measure',
POSITIVE_RATIO_MEASURE(7850.),#1238);
#1247=PROPERTY_DEFINITION_REPRESENTATION(#1287,#1263);
#1248=PROPERTY_DEFINITION_REPRESENTATION(#1288,#1264);
#1249=PROPERTY_DEFINITION_REPRESENTATION(#1289,#1265);
#1250=PROPERTY_DEFINITION_REPRESENTATION(#1290,#1266);
#1251=PROPERTY_DEFINITION_REPRESENTATION(#1291,#1267);
#1252=PROPERTY_DEFINITION_REPRESENTATION(#1292,#1268);
#1253=PROPERTY_DEFINITION_REPRESENTATION(#1293,#1269);
#1254=PROPERTY_DEFINITION_REPRESENTATION(#1294,#1270);
#1255=PROPERTY_DEFINITION_REPRESENTATION(#1295,#1271);
#1256=PROPERTY_DEFINITION_REPRESENTATION(#1296,#1272);
#1257=PROPERTY_DEFINITION_REPRESENTATION(#1297,#1273);
#1258=PROPERTY_DEFINITION_REPRESENTATION(#1298,#1274);
#1259=PROPERTY_DEFINITION_REPRESENTATION(#1299,#1275);
#1260=PROPERTY_DEFINITION_REPRESENTATION(#1300,#1276);
#1261=PROPERTY_DEFINITION_REPRESENTATION(#1301,#1277);
#1262=PROPERTY_DEFINITION_REPRESENTATION(#1302,#1278);
#1263=REPRESENTATION('material name',(#1279),#2230);
#1264=REPRESENTATION('density',(#1239),#2230);
#1265=REPRESENTATION('material name',(#1280),#2231);
#1266=REPRESENTATION('density',(#1240),#2231);
#1267=REPRESENTATION('material name',(#1281),#2232);
#1268=REPRESENTATION('density',(#1241),#2232);
#1269=REPRESENTATION('material name',(#1282),#2233);
#1270=REPRESENTATION('density',(#1242),#2233);
#1271=REPRESENTATION('material name',(#1283),#2234);
#1272=REPRESENTATION('density',(#1243),#2234);
#1273=REPRESENTATION('material name',(#1284),#2235);
#1274=REPRESENTATION('density',(#1244),#2235);
#1275=REPRESENTATION('material name',(#1285),#2236);
#1276=REPRESENTATION('density',(#1245),#2236);
#1277=REPRESENTATION('material name',(#1286),#2237);
#1278=REPRESENTATION('density',(#1246),#2237);
#1279=DESCRIPTIVE_REPRESENTATION_ITEM('Steel','Steel');
#1280=DESCRIPTIVE_REPRESENTATION_ITEM('Steel','Steel');
#1281=DESCRIPTIVE_REPRESENTATION_ITEM('Steel','Steel');
#1282=DESCRIPTIVE_REPRESENTATION_ITEM('Steel','Steel');
#1283=DESCRIPTIVE_REPRESENTATION_ITEM('Steel','Steel');
#1284=DESCRIPTIVE_REPRESENTATION_ITEM('Steel','Steel');
#1285=DESCRIPTIVE_REPRESENTATION_ITEM('Steel','Steel');
#1286=DESCRIPTIVE_REPRESENTATION_ITEM('Steel','Steel');
#1287=PROPERTY_DEFINITION('material property','material name',#2280);
#1288=PROPERTY_DEFINITION('material property','density of part',#2280);
#1289=PROPERTY_DEFINITION('material property','material name',#2281);
#1290=PROPERTY_DEFINITION('material property','density of part',#2281);
#1291=PROPERTY_DEFINITION('material property','material name',#2282);
#1292=PROPERTY_DEFINITION('material property','density of part',#2282);
#1293=PROPERTY_DEFINITION('material property','material name',#2283);
#1294=PROPERTY_DEFINITION('material property','density of part',#2283);
#1295=PROPERTY_DEFINITION('material property','material name',#2284);
#1296=PROPERTY_DEFINITION('material property','density of part',#2284);
#1297=PROPERTY_DEFINITION('material property','material name',#2285);
#1298=PROPERTY_DEFINITION('material property','density of part',#2285);
#1299=PROPERTY_DEFINITION('material property','material name',#2286);
#1300=PROPERTY_DEFINITION('material property','density of part',#2286);
#1301=PROPERTY_DEFINITION('material property','material name',#2287);
#1302=PROPERTY_DEFINITION('material property','density of part',#2287);
#1303=AXIS2_PLACEMENT_3D('',#1868,#1463,#1464);
#1304=AXIS2_PLACEMENT_3D('',#1869,#1465,#1466);
#1305=AXIS2_PLACEMENT_3D('',#1870,#1467,#1468);
#1306=AXIS2_PLACEMENT_3D('',#1872,#1469,#1470);
#1307=AXIS2_PLACEMENT_3D('',#1875,#1472,#1473);
#1308=AXIS2_PLACEMENT_3D('',#1876,#1474,#1475);
#1309=AXIS2_PLACEMENT_3D('',#1881,#1477,#1478);
#1310=AXIS2_PLACEMENT_3D('',#1884,#1480,#1481);
#1311=AXIS2_PLACEMENT_3D('',#1885,#1482,#1483);
#1312=AXIS2_PLACEMENT_3D('',#1890,#1485,#1486);
#1313=AXIS2_PLACEMENT_3D('',#1893,#1488,#1489);
#1314=AXIS2_PLACEMENT_3D('',#1894,#1490,#1491);
#1315=AXIS2_PLACEMENT_3D('',#1899,#1493,#1494);
#1316=AXIS2_PLACEMENT_3D('',#1902,#1496,#1497);
#1317=AXIS2_PLACEMENT_3D('',#1903,#1498,#1499);
#1318=AXIS2_PLACEMENT_3D('',#1908,#1501,#1502);
#1319=AXIS2_PLACEMENT_3D('',#1911,#1504,#1505);
#1320=AXIS2_PLACEMENT_3D('',#1912,#1506,#1507);
#1321=AXIS2_PLACEMENT_3D('',#1917,#1509,#1510);
#1322=AXIS2_PLACEMENT_3D('',#1920,#1512,#1513);
#1323=AXIS2_PLACEMENT_3D('',#1921,#1514,#1515);
#1324=AXIS2_PLACEMENT_3D('',#1923,#1516,#1517);
#1325=AXIS2_PLACEMENT_3D('',#1926,#1519,#1520);
#1326=AXIS2_PLACEMENT_3D('',#1927,#1521,#1522);
#1327=AXIS2_PLACEMENT_3D('',#1929,#1523,#1524);
#1328=AXIS2_PLACEMENT_3D('',#1932,#1526,#1527);
#1329=AXIS2_PLACEMENT_3D('',#1933,#1528,#1529);
#1330=AXIS2_PLACEMENT_3D('',#1935,#1530,#1531);
#1331=AXIS2_PLACEMENT_3D('',#1938,#1533,#1534);
#1332=AXIS2_PLACEMENT_3D('',#1939,#1535,#1536);
#1333=AXIS2_PLACEMENT_3D('',#1941,#1537,#1538);
#1334=AXIS2_PLACEMENT_3D('',#1944,#1540,#1541);
#1335=AXIS2_PLACEMENT_3D('',#1945,#1542,#1543);
#1336=AXIS2_PLACEMENT_3D('',#1949,#1545,#1546);
#1337=AXIS2_PLACEMENT_3D('',#1952,#1548,#1549);
#1338=AXIS2_PLACEMENT_3D('',#1956,#1551,#1552);
#1339=AXIS2_PLACEMENT_3D('',#1959,#1554,#1555);
#1340=AXIS2_PLACEMENT_3D('',#1963,#1557,#1558);
#1341=AXIS2_PLACEMENT_3D('',#1966,#1560,#1561);
#1342=AXIS2_PLACEMENT_3D('',#1970,#1563,#1564);
#1343=AXIS2_PLACEMENT_3D('',#1973,#1566,#1567);
#1344=AXIS2_PLACEMENT_3D('',#1975,#1568,#1569);
#1345=AXIS2_PLACEMENT_3D('',#1979,#1571,#1572);
#1346=AXIS2_PLACEMENT_3D('',#1983,#1574,#1575);
#1347=AXIS2_PLACEMENT_3D('',#1985,#1576,#1577);
#1348=AXIS2_PLACEMENT_3D('',#1987,#1578,#1579);
#1349=AXIS2_PLACEMENT_3D('',#1991,#1581,#1582);
#1350=AXIS2_PLACEMENT_3D('',#1994,#1584,#1585);
#1351=AXIS2_PLACEMENT_3D('',#1995,#1586,#1587);
#1352=AXIS2_PLACEMENT_3D('',#1997,#1588,#1589);
#1353=AXIS2_PLACEMENT_3D('',#1999,#1591,#1592);
#1354=AXIS2_PLACEMENT_3D('',#2004,#1595,#1596);
#1355=AXIS2_PLACEMENT_3D('',#2005,#1597,#1598);
#1356=AXIS2_PLACEMENT_3D('',#2007,#1599,#1600);
#1357=AXIS2_PLACEMENT_3D('',#2011,#1602,#1603);
#1358=AXIS2_PLACEMENT_3D('',#2014,#1605,#1606);
#1359=AXIS2_PLACEMENT_3D('',#2016,#1607,#1608);
#1360=AXIS2_PLACEMENT_3D('',#2020,#1610,#1611);
#1361=AXIS2_PLACEMENT_3D('',#2023,#1613,#1614);
#1362=AXIS2_PLACEMENT_3D('',#2027,#1616,#1617);
#1363=AXIS2_PLACEMENT_3D('',#2030,#1619,#1620);
#1364=AXIS2_PLACEMENT_3D('',#2034,#1622,#1623);
#1365=AXIS2_PLACEMENT_3D('',#2037,#1625,#1626);
#1366=AXIS2_PLACEMENT_3D('',#2041,#1628,#1629);
#1367=AXIS2_PLACEMENT_3D('',#2044,#1631,#1632);
#1368=AXIS2_PLACEMENT_3D('',#2048,#1634,#1635);
#1369=AXIS2_PLACEMENT_3D('',#2050,#1637,#1638);
#1370=AXIS2_PLACEMENT_3D('',#2052,#1640,#1641);
#1371=AXIS2_PLACEMENT_3D('',#2054,#1643,#1644);
#1372=AXIS2_PLACEMENT_3D('',#2056,#1646,#1647);
#1373=AXIS2_PLACEMENT_3D('',#2058,#1649,#1650);
#1374=AXIS2_PLACEMENT_3D('',#2060,#1652,#1653);
#1375=AXIS2_PLACEMENT_3D('',#2061,#1654,#1655);
#1376=AXIS2_PLACEMENT_3D('',#2063,#1657,#1658);
#1377=AXIS2_PLACEMENT_3D('',#2065,#1660,#1661);
#1378=AXIS2_PLACEMENT_3D('',#2067,#1663,#1664);
#1379=AXIS2_PLACEMENT_3D('',#2068,#1665,#1666);
#1380=AXIS2_PLACEMENT_3D('',#2070,#1668,#1669);
#1381=AXIS2_PLACEMENT_3D('',#2072,#1671,#1672);
#1382=AXIS2_PLACEMENT_3D('',#2075,#1675,#1676);
#1383=AXIS2_PLACEMENT_3D('',#2077,#1678,#1679);
#1384=AXIS2_PLACEMENT_3D('',#2078,#1680,#1681);
#1385=AXIS2_PLACEMENT_3D('',#2080,#1683,#1684);
#1386=AXIS2_PLACEMENT_3D('',#2082,#1686,#1687);
#1387=AXIS2_PLACEMENT_3D('',#2083,#1688,#1689);
#1388=AXIS2_PLACEMENT_3D('',#2084,#1690,#1691);
#1389=AXIS2_PLACEMENT_3D('',#2086,#1693,#1694);
#1390=AXIS2_PLACEMENT_3D('',#2088,#1696,#1697);
#1391=AXIS2_PLACEMENT_3D('',#2090,#1699,#1700);
#1392=AXIS2_PLACEMENT_3D('',#2091,#1701,#1702);
#1393=AXIS2_PLACEMENT_3D('',#2093,#1704,#1705);
#1394=AXIS2_PLACEMENT_3D('',#2094,#1706,#1707);
#1395=AXIS2_PLACEMENT_3D('',#2095,#1708,#1709);
#1396=AXIS2_PLACEMENT_3D('',#2097,#1710,#1711);
#1397=AXIS2_PLACEMENT_3D('',#2098,#1712,#1713);
#1398=AXIS2_PLACEMENT_3D('',#2101,#1715,#1716);
#1399=AXIS2_PLACEMENT_3D('',#2102,#1717,#1718);
#1400=AXIS2_PLACEMENT_3D('',#2103,#1719,#1720);
#1401=AXIS2_PLACEMENT_3D('',#2104,#1721,#1722);
#1402=AXIS2_PLACEMENT_3D('',#2106,#1723,#1724);
#1403=AXIS2_PLACEMENT_3D('',#2107,#1725,#1726);
#1404=AXIS2_PLACEMENT_3D('',#2110,#1728,#1729);
#1405=AXIS2_PLACEMENT_3D('',#2111,#1730,#1731);
#1406=AXIS2_PLACEMENT_3D('',#2112,#1732,#1733);
#1407=AXIS2_PLACEMENT_3D('',#2113,#1734,#1735);
#1408=AXIS2_PLACEMENT_3D('',#2115,#1736,#1737);
#1409=AXIS2_PLACEMENT_3D('',#2118,#1739,#1740);
#1410=AXIS2_PLACEMENT_3D('',#2119,#1741,#1742);
#1411=AXIS2_PLACEMENT_3D('',#2121,#1743,#1744);
#1412=AXIS2_PLACEMENT_3D('',#2122,#1745,#1746);
#1413=AXIS2_PLACEMENT_3D('',#2125,#1748,#1749);
#1414=AXIS2_PLACEMENT_3D('',#2126,#1750,#1751);
#1415=AXIS2_PLACEMENT_3D('',#2127,#1752,#1753);
#1416=AXIS2_PLACEMENT_3D('',#2128,#1754,#1755);
#1417=AXIS2_PLACEMENT_3D('',#2130,#1756,#1757);
#1418=AXIS2_PLACEMENT_3D('',#2132,#1758,#1759);
#1419=AXIS2_PLACEMENT_3D('',#2133,#1760,#1761);
#1420=AXIS2_PLACEMENT_3D('',#2136,#1763,#1764);
#1421=AXIS2_PLACEMENT_3D('',#2137,#1765,#1766);
#1422=AXIS2_PLACEMENT_3D('',#2139,#1767,#1768);
#1423=AXIS2_PLACEMENT_3D('',#2141,#1770,#1771);
#1424=AXIS2_PLACEMENT_3D('',#2142,#1772,#1773);
#1425=AXIS2_PLACEMENT_3D('',#2143,#1774,#1775);
#1426=AXIS2_PLACEMENT_3D('',#2145,#1776,#1777);
#1427=AXIS2_PLACEMENT_3D('',#2148,#1779,#1780);
#1428=AXIS2_PLACEMENT_3D('',#2149,#1781,#1782);
#1429=AXIS2_PLACEMENT_3D('',#2151,#1783,#1784);
#1430=AXIS2_PLACEMENT_3D('',#2154,#1786,#1787);
#1431=AXIS2_PLACEMENT_3D('',#2155,#1788,#1789);
#1432=AXIS2_PLACEMENT_3D('',#2157,#1790,#1791);
#1433=AXIS2_PLACEMENT_3D('',#2160,#1793,#1794);
#1434=AXIS2_PLACEMENT_3D('',#2161,#1795,#1796);
#1435=AXIS2_PLACEMENT_3D('',#2162,#1797,#1798);
#1436=AXIS2_PLACEMENT_3D('',#2163,#1799,#1800);
#1437=AXIS2_PLACEMENT_3D('',#2164,#1801,#1802);
#1438=AXIS2_PLACEMENT_3D('',#2166,#1803,#1804);
#1439=AXIS2_PLACEMENT_3D('',#2167,#1805,#1806);
#1440=AXIS2_PLACEMENT_3D('',#2170,#1808,#1809);
#1441=AXIS2_PLACEMENT_3D('',#2171,#1810,#1811);
#1442=AXIS2_PLACEMENT_3D('',#2172,#1812,#1813);
#1443=AXIS2_PLACEMENT_3D('',#2173,#1814,#1815);
#1444=AXIS2_PLACEMENT_3D('',#2175,#1816,#1817);
#1445=AXIS2_PLACEMENT_3D('',#2178,#1819,#1820);
#1446=AXIS2_PLACEMENT_3D('',#2179,#1821,#1822);
#1447=AXIS2_PLACEMENT_3D('',#2181,#1823,#1824);
#1448=AXIS2_PLACEMENT_3D('',#2184,#1826,#1827);
#1449=AXIS2_PLACEMENT_3D('',#2185,#1828,#1829);
#1450=AXIS2_PLACEMENT_3D('',#2194,#1834,#1835);
#1451=AXIS2_PLACEMENT_3D('',#2200,#1839,#1840);
#1452=AXIS2_PLACEMENT_3D('',#2204,#1843,#1844);
#1453=AXIS2_PLACEMENT_3D('',#2208,#1847,#1848);
#1454=AXIS2_PLACEMENT_3D('',#2210,#1850,#1851);
#1455=AXIS2_PLACEMENT_3D('',#2211,#1852,#1853);
#1456=AXIS2_PLACEMENT_3D('',#2212,#1854,#1855);
#1457=AXIS2_PLACEMENT_3D('',#2213,#1856,#1857);
#1458=AXIS2_PLACEMENT_3D('',#2214,#1858,#1859);
#1459=AXIS2_PLACEMENT_3D('',#2215,#1860,#1861);
#1460=AXIS2_PLACEMENT_3D('',#2216,#1862,#1863);
#1461=AXIS2_PLACEMENT_3D('',#2217,#1864,#1865);
#1462=AXIS2_PLACEMENT_3D('',#2218,#1866,#1867);
#1463=DIRECTION('axis',(0.,0.,1.));
#1464=DIRECTION('refdir',(1.,0.,0.));
#1465=DIRECTION('axis',(0.,0.,1.));
#1466=DIRECTION('refdir',(1.,0.,0.));
#1467=DIRECTION('center_axis',(0.,-1.,0.));
#1468=DIRECTION('ref_axis',(1.,0.,0.));
#1469=DIRECTION('center_axis',(0.,-1.,0.));
#1470=DIRECTION('ref_axis',(1.,0.,0.));
#1471=DIRECTION('',(0.,-1.,0.));
#1472=DIRECTION('center_axis',(0.,1.,0.));
#1473=DIRECTION('ref_axis',(1.,0.,0.));
#1474=DIRECTION('center_axis',(0.,-1.,0.));
#1475=DIRECTION('ref_axis',(0.499999999999999,0.,-0.866025403784439));
#1476=DIRECTION('',(0.,1.,0.));
#1477=DIRECTION('center_axis',(0.,1.,0.));
#1478=DIRECTION('ref_axis',(0.499999999999999,0.,-0.866025403784439));
#1479=DIRECTION('',(0.,-1.,0.));
#1480=DIRECTION('center_axis',(0.,-1.,0.));
#1481=DIRECTION('ref_axis',(0.499999999999999,0.,-0.866025403784439));
#1482=DIRECTION('center_axis',(0.,-1.,0.));
#1483=DIRECTION('ref_axis',(-0.5,0.,-0.866025403784438));
#1484=DIRECTION('',(0.,1.,0.));
#1485=DIRECTION('center_axis',(0.,1.,0.));
#1486=DIRECTION('ref_axis',(-0.5,0.,-0.866025403784438));
#1487=DIRECTION('',(0.,-1.,0.));
#1488=DIRECTION('center_axis',(0.,-1.,0.));
#1489=DIRECTION('ref_axis',(-0.5,0.,-0.866025403784438));
#1490=DIRECTION('center_axis',(0.,-1.,0.));
#1491=DIRECTION('ref_axis',(-1.,0.,8.54017711250121E-17));
#1492=DIRECTION('',(0.,1.,0.));
#1493=DIRECTION('center_axis',(0.,1.,0.));
#1494=DIRECTION('ref_axis',(-1.,0.,8.54017711250121E-17));
#1495=DIRECTION('',(0.,-1.,0.));
#1496=DIRECTION('center_axis',(0.,-1.,0.));
#1497=DIRECTION('ref_axis',(-1.,0.,8.54017711250121E-17));
#1498=DIRECTION('center_axis',(0.,-1.,0.));
#1499=DIRECTION('ref_axis',(-0.5,0.,0.866025403784439));
#1500=DIRECTION('',(0.,1.,0.));
#1501=DIRECTION('center_axis',(0.,1.,0.));
#1502=DIRECTION('ref_axis',(-0.5,0.,0.866025403784439));
#1503=DIRECTION('',(0.,-1.,0.));
#1504=DIRECTION('center_axis',(0.,-1.,0.));
#1505=DIRECTION('ref_axis',(-0.5,0.,0.866025403784439));
#1506=DIRECTION('center_axis',(0.,-1.,0.));
#1507=DIRECTION('ref_axis',(0.5,0.,0.866025403784439));
#1508=DIRECTION('',(0.,1.,0.));
#1509=DIRECTION('center_axis',(0.,1.,0.));
#1510=DIRECTION('ref_axis',(0.5,0.,0.866025403784439));
#1511=DIRECTION('',(0.,-1.,0.));
#1512=DIRECTION('center_axis',(0.,-1.,0.));
#1513=DIRECTION('ref_axis',(0.5,0.,0.866025403784439));
#1514=DIRECTION('center_axis',(0.,-1.,0.));
#1515=DIRECTION('ref_axis',(-1.,0.,0.));
#1516=DIRECTION('center_axis',(0.,-1.,0.));
#1517=DIRECTION('ref_axis',(-1.,0.,0.));
#1518=DIRECTION('',(0.,-1.,0.));
#1519=DIRECTION('center_axis',(0.,1.,0.));
#1520=DIRECTION('ref_axis',(-1.,0.,0.));
#1521=DIRECTION('center_axis',(0.,1.,0.));
#1522=DIRECTION('ref_axis',(-1.,0.,0.));
#1523=DIRECTION('center_axis',(0.,1.,0.));
#1524=DIRECTION('ref_axis',(-1.,0.,0.));
#1525=DIRECTION('',(0.,-1.,0.));
#1526=DIRECTION('center_axis',(0.,-1.,0.));
#1527=DIRECTION('ref_axis',(-1.,0.,0.));
#1528=DIRECTION('center_axis',(0.,-1.,0.));
#1529=DIRECTION('ref_axis',(1.,0.,0.));
#1530=DIRECTION('center_axis',(0.,-1.,0.));
#1531=DIRECTION('ref_axis',(1.,0.,0.));
#1532=DIRECTION('',(0.,-1.,0.));
#1533=DIRECTION('center_axis',(0.,1.,0.));
#1534=DIRECTION('ref_axis',(1.,0.,0.));
#1535=DIRECTION('center_axis',(0.,-1.,0.));
#1536=DIRECTION('ref_axis',(1.,0.,0.));
#1537=DIRECTION('center_axis',(0.,-1.,0.));
#1538=DIRECTION('ref_axis',(1.,0.,0.));
#1539=DIRECTION('',(0.,-1.,0.));
#1540=DIRECTION('center_axis',(0.,1.,0.));
#1541=DIRECTION('ref_axis',(1.,0.,0.));
#1542=DIRECTION('center_axis',(0.,1.,0.));
#1543=DIRECTION('ref_axis',(1.,0.,0.));
#1544=DIRECTION('',(-1.,0.,0.));
#1545=DIRECTION('center_axis',(0.,-1.,0.));
#1546=DIRECTION('ref_axis',(-8.88178419700125E-16,0.,-1.));
#1547=DIRECTION('',(-1.,0.,0.));
#1548=DIRECTION('center_axis',(0.,-1.,0.));
#1549=DIRECTION('ref_axis',(-1.,0.,0.));
#1550=DIRECTION('',(0.5,0.,-0.866025403784439));
#1551=DIRECTION('center_axis',(0.,-1.,0.));
#1552=DIRECTION('ref_axis',(-0.866025403784439,0.,-0.5));
#1553=DIRECTION('',(-0.5,0.,0.866025403784439));
#1554=DIRECTION('center_axis',(0.,1.,0.));
#1555=DIRECTION('ref_axis',(1.,0.,0.));
#1556=DIRECTION('',(0.5,0.,0.866025403784439));
#1557=DIRECTION('center_axis',(0.,1.,0.));
#1558=DIRECTION('ref_axis',(0.866025403784439,0.,-0.5));
#1559=DIRECTION('',(-0.5,0.,-0.866025403784439));
#1560=DIRECTION('center_axis',(0.,1.,0.));
#1561=DIRECTION('ref_axis',(1.,0.,0.));
#1562=DIRECTION('',(1.,0.,0.));
#1563=DIRECTION('center_axis',(0.,1.,0.));
#1564=DIRECTION('ref_axis',(8.88178419700125E-16,0.,-1.));
#1565=DIRECTION('',(1.,0.,0.));
#1566=DIRECTION('center_axis',(0.,-1.,0.));
#1567=DIRECTION('ref_axis',(1.,0.,0.));
#1568=DIRECTION('center_axis',(0.,-1.,0.));
#1569=DIRECTION('ref_axis',(1.,0.,0.));
#1570=DIRECTION('',(-0.5,0.,0.866025403784439));
#1571=DIRECTION('center_axis',(0.,-1.,0.));
#1572=DIRECTION('ref_axis',(0.866025403784439,0.,0.5));
#1573=DIRECTION('',(0.5,0.,-0.866025403784439));
#1574=DIRECTION('center_axis',(0.,-1.,0.));
#1575=DIRECTION('ref_axis',(1.,0.,0.));
#1576=DIRECTION('center_axis',(0.,-1.,0.));
#1577=DIRECTION('ref_axis',(1.,0.,0.));
#1578=DIRECTION('center_axis',(0.,-1.,0.));
#1579=DIRECTION('ref_axis',(1.,0.,0.));
#1580=DIRECTION('',(-0.5,0.,-0.866025403784439));
#1581=DIRECTION('center_axis',(0.,1.,0.));
#1582=DIRECTION('ref_axis',(-0.866025403784439,0.,0.5));
#1583=DIRECTION('',(0.5,0.,0.866025403784439));
#1584=DIRECTION('center_axis',(0.,1.,0.));
#1585=DIRECTION('ref_axis',(-1.,0.,0.));
#1586=DIRECTION('center_axis',(0.,1.,0.));
#1587=DIRECTION('ref_axis',(1.,0.,0.));
#1588=DIRECTION('center_axis',(0.,1.,0.));
#1589=DIRECTION('ref_axis',(1.,0.,0.));
#1590=DIRECTION('',(0.,-1.,0.));
#1591=DIRECTION('center_axis',(0.,-1.,0.));
#1592=DIRECTION('ref_axis',(1.,0.,0.));
#1593=DIRECTION('',(0.,-1.,0.));
#1594=DIRECTION('',(0.,1.,0.));
#1595=DIRECTION('center_axis',(0.,1.,0.));
#1596=DIRECTION('ref_axis',(1.,0.,0.));
#1597=DIRECTION('center_axis',(0.,1.,0.));
#1598=DIRECTION('ref_axis',(1.,0.,0.));
#1599=DIRECTION('center_axis',(0.,-1.,0.));
#1600=DIRECTION('ref_axis',(-1.,0.,0.));
#1601=DIRECTION('',(0.5,0.,0.866025403784439));
#1602=DIRECTION('center_axis',(0.,1.,0.));
#1603=DIRECTION('ref_axis',(-0.866025403784439,0.,0.5));
#1604=DIRECTION('',(-0.5,0.,-0.866025403784439));
#1605=DIRECTION('center_axis',(0.,1.,0.));
#1606=DIRECTION('ref_axis',(1.,0.,0.));
#1607=DIRECTION('center_axis',(0.,1.,0.));
#1608=DIRECTION('ref_axis',(1.,0.,0.));
#1609=DIRECTION('',(0.5,0.,-0.866025403784439));
#1610=DIRECTION('center_axis',(0.,-1.,0.));
#1611=DIRECTION('ref_axis',(0.866025403784439,0.,0.5));
#1612=DIRECTION('',(-0.5,0.,0.866025403784439));
#1613=DIRECTION('center_axis',(0.,1.,0.));
#1614=DIRECTION('ref_axis',(1.,0.,0.));
#1615=DIRECTION('',(1.,0.,0.));
#1616=DIRECTION('center_axis',(0.,-1.,0.));
#1617=DIRECTION('ref_axis',(8.88178419700125E-16,0.,1.));
#1618=DIRECTION('',(1.,0.,0.));
#1619=DIRECTION('center_axis',(0.,-1.,0.));
#1620=DIRECTION('ref_axis',(1.,0.,0.));
#1621=DIRECTION('',(-0.5,0.,-0.866025403784439));
#1622=DIRECTION('center_axis',(0.,1.,0.));
#1623=DIRECTION('ref_axis',(0.866025403784439,0.,-0.5));
#1624=DIRECTION('',(0.5,0.,0.866025403784439));
#1625=DIRECTION('center_axis',(0.,-1.,0.));
#1626=DIRECTION('ref_axis',(1.,0.,0.));
#1627=DIRECTION('',(-0.5,0.,0.866025403784439));
#1628=DIRECTION('center_axis',(0.,-1.,0.));
#1629=DIRECTION('ref_axis',(-0.866025403784439,0.,-0.5));
#1630=DIRECTION('',(0.5,0.,-0.866025403784439));
#1631=DIRECTION('center_axis',(0.,1.,0.));
#1632=DIRECTION('ref_axis',(-1.,0.,0.));
#1633=DIRECTION('',(-1.,0.,0.));
#1634=DIRECTION('center_axis',(0.,1.,0.));
#1635=DIRECTION('ref_axis',(-8.88178419700125E-16,0.,1.));
#1636=DIRECTION('',(-1.,0.,0.));
#1637=DIRECTION('center_axis',(0.,1.,0.));
#1638=DIRECTION('ref_axis',(1.,0.,0.));
#1639=DIRECTION('',(0.,-1.,0.));
#1640=DIRECTION('center_axis',(0.,1.,0.));
#1641=DIRECTION('ref_axis',(1.,0.,0.));
#1642=DIRECTION('',(0.,-1.,0.));
#1643=DIRECTION('center_axis',(-0.866025403784439,0.,0.5));
#1644=DIRECTION('ref_axis',(-0.5,0.,-0.866025403784439));
#1645=DIRECTION('',(0.,-1.,0.));
#1646=DIRECTION('center_axis',(0.,-1.,0.));
#1647=DIRECTION('ref_axis',(-0.866025403784439,0.,0.5));
#1648=DIRECTION('',(0.,-1.,0.));
#1649=DIRECTION('center_axis',(0.866025403784439,0.,-0.5));
#1650=DIRECTION('ref_axis',(0.5,0.,0.866025403784439));
#1651=DIRECTION('',(0.,-1.,0.));
#1652=DIRECTION('center_axis',(0.,-1.,0.));
#1653=DIRECTION('ref_axis',(-1.,0.,0.));
#1654=DIRECTION('center_axis',(0.,0.,1.));
#1655=DIRECTION('ref_axis',(-1.,0.,0.));
#1656=DIRECTION('',(0.,-1.,0.));
#1657=DIRECTION('center_axis',(-0.866025403784439,0.,-0.5));
#1658=DIRECTION('ref_axis',(0.5,0.,-0.866025403784439));
#1659=DIRECTION('',(0.,-1.,0.));
#1660=DIRECTION('center_axis',(0.,1.,0.));
#1661=DIRECTION('ref_axis',(0.866025403784439,0.,0.5));
#1662=DIRECTION('',(0.,-1.,0.));
#1663=DIRECTION('center_axis',(0.866025403784439,0.,0.5));
#1664=DIRECTION('ref_axis',(-0.5,0.,0.866025403784439));
#1665=DIRECTION('center_axis',(0.,1.,0.));
#1666=DIRECTION('ref_axis',(1.,0.,0.));
#1667=DIRECTION('',(0.,-1.,0.));
#1668=DIRECTION('center_axis',(0.,0.,-1.));
#1669=DIRECTION('ref_axis',(1.,0.,0.));
#1670=DIRECTION('',(0.,-1.,0.));
#1671=DIRECTION('center_axis',(0.866025403784439,0.,0.5));
#1672=DIRECTION('ref_axis',(-0.5,0.,0.866025403784439));
#1673=DIRECTION('',(0.,-1.,0.));
#1674=DIRECTION('',(0.,-1.,0.));
#1675=DIRECTION('center_axis',(0.,1.,0.));
#1676=DIRECTION('ref_axis',(-0.866025403784439,0.,-0.5));
#1677=DIRECTION('',(0.,-1.,0.));
#1678=DIRECTION('center_axis',(-0.866025403784439,0.,-0.5));
#1679=DIRECTION('ref_axis',(0.5,0.,-0.866025403784439));
#1680=DIRECTION('center_axis',(0.,1.,0.));
#1681=DIRECTION('ref_axis',(-1.,0.,0.));
#1682=DIRECTION('',(0.,-1.,0.));
#1683=DIRECTION('center_axis',(0.,0.,1.));
#1684=DIRECTION('ref_axis',(-1.,0.,0.));
#1685=DIRECTION('',(0.,-1.,0.));
#1686=DIRECTION('center_axis',(0.,1.,0.));
#1687=DIRECTION('ref_axis',(-8.88178419700125E-16,0.,-1.));
#1688=DIRECTION('center_axis',(0.,-1.,0.));
#1689=DIRECTION('ref_axis',(1.,0.,0.));
#1690=DIRECTION('center_axis',(0.866025403784439,0.,-0.5));
#1691=DIRECTION('ref_axis',(0.5,0.,0.866025403784439));
#1692=DIRECTION('',(0.,-1.,0.));
#1693=DIRECTION('center_axis',(0.,-1.,0.));
#1694=DIRECTION('ref_axis',(0.866025403784439,0.,-0.5));
#1695=DIRECTION('',(0.,-1.,0.));
#1696=DIRECTION('center_axis',(-0.866025403784439,0.,0.5));
#1697=DIRECTION('ref_axis',(-0.5,0.,-0.866025403784439));
#1698=DIRECTION('',(0.,-1.,0.));
#1699=DIRECTION('center_axis',(0.,-1.,0.));
#1700=DIRECTION('ref_axis',(1.,0.,0.));
#1701=DIRECTION('center_axis',(0.,0.,-1.));
#1702=DIRECTION('ref_axis',(1.,0.,0.));
#1703=DIRECTION('',(0.,-1.,0.));
#1704=DIRECTION('center_axis',(0.,-1.,0.));
#1705=DIRECTION('ref_axis',(8.88178419700125E-16,0.,-1.));
#1706=DIRECTION('axis',(0.,0.,1.));
#1707=DIRECTION('refdir',(1.,0.,0.));
#1708=DIRECTION('center_axis',(0.,1.,0.));
#1709=DIRECTION('ref_axis',(1.,0.,0.));
#1710=DIRECTION('center_axis',(0.,-1.,0.));
#1711=DIRECTION('ref_axis',(1.,0.,0.));
#1712=DIRECTION('center_axis',(0.,-1.,0.));
#1713=DIRECTION('ref_axis',(1.,0.,0.));
#1714=DIRECTION('',(0.,1.,0.));
#1715=DIRECTION('center_axis',(0.,-1.,0.));
#1716=DIRECTION('ref_axis',(1.,0.,0.));
#1717=DIRECTION('center_axis',(0.,1.,0.));
#1718=DIRECTION('ref_axis',(1.,0.,0.));
#1719=DIRECTION('axis',(0.,0.,1.));
#1720=DIRECTION('refdir',(1.,0.,0.));
#1721=DIRECTION('center_axis',(0.,-1.,0.));
#1722=DIRECTION('ref_axis',(1.,0.,0.));
#1723=DIRECTION('center_axis',(0.,-1.,0.));
#1724=DIRECTION('ref_axis',(1.,0.,0.));
#1725=DIRECTION('center_axis',(0.,-1.,0.));
#1726=DIRECTION('ref_axis',(1.,0.,0.));
#1727=DIRECTION('',(0.,1.,0.));
#1728=DIRECTION('center_axis',(0.,-1.,0.));
#1729=DIRECTION('ref_axis',(1.,0.,0.));
#1730=DIRECTION('center_axis',(0.,1.,0.));
#1731=DIRECTION('ref_axis',(0.,0.,1.));
#1732=DIRECTION('axis',(0.,0.,1.));
#1733=DIRECTION('refdir',(1.,0.,0.));
#1734=DIRECTION('center_axis',(0.,1.,0.));
#1735=DIRECTION('ref_axis',(1.,0.,0.));
#1736=DIRECTION('center_axis',(0.,-1.,0.));
#1737=DIRECTION('ref_axis',(1.,0.,0.));
#1738=DIRECTION('',(0.,-1.,0.));
#1739=DIRECTION('center_axis',(0.,1.,0.));
#1740=DIRECTION('ref_axis',(1.,0.,0.));
#1741=DIRECTION('center_axis',(0.,1.,0.));
#1742=DIRECTION('ref_axis',(1.,0.,0.));
#1743=DIRECTION('center_axis',(0.,-1.,0.));
#1744=DIRECTION('ref_axis',(1.,0.,0.));
#1745=DIRECTION('center_axis',(0.,-1.,0.));
#1746=DIRECTION('ref_axis',(1.,0.,0.));
#1747=DIRECTION('',(0.,1.,0.));
#1748=DIRECTION('center_axis',(0.,-1.,0.));
#1749=DIRECTION('ref_axis',(1.,0.,0.));
#1750=DIRECTION('center_axis',(0.,1.,0.));
#1751=DIRECTION('ref_axis',(1.,0.,0.));
#1752=DIRECTION('axis',(0.,0.,1.));
#1753=DIRECTION('refdir',(1.,0.,0.));
#1754=DIRECTION('center_axis',(0.,-1.,0.));
#1755=DIRECTION('ref_axis',(1.,0.,0.));
#1756=DIRECTION('center_axis',(0.,-1.,0.));
#1757=DIRECTION('ref_axis',(1.,0.,0.));
#1758=DIRECTION('center_axis',(0.,-1.,0.));
#1759=DIRECTION('ref_axis',(1.,0.,0.));
#1760=DIRECTION('center_axis',(0.,-1.,0.));
#1761=DIRECTION('ref_axis',(1.,0.,0.));
#1762=DIRECTION('',(0.,1.,0.));
#1763=DIRECTION('center_axis',(0.,1.,0.));
#1764=DIRECTION('ref_axis',(1.,0.,0.));
#1765=DIRECTION('center_axis',(0.,-1.,0.));
#1766=DIRECTION('ref_axis',(1.,0.,0.));
#1767=DIRECTION('center_axis',(0.,-1.,0.));
#1768=DIRECTION('ref_axis',(1.,0.,0.));
#1769=DIRECTION('',(0.,-1.,0.));
#1770=DIRECTION('center_axis',(0.,1.,0.));
#1771=DIRECTION('ref_axis',(0.,0.,1.));
#1772=DIRECTION('axis',(0.,0.,1.));
#1773=DIRECTION('refdir',(1.,0.,0.));
#1774=DIRECTION('center_axis',(0.,-1.,0.));
#1775=DIRECTION('ref_axis',(1.,0.,0.));
#1776=DIRECTION('center_axis',(0.,-1.,0.));
#1777=DIRECTION('ref_axis',(1.,0.,0.));
#1778=DIRECTION('',(0.,-1.,0.));
#1779=DIRECTION('center_axis',(0.,1.,0.));
#1780=DIRECTION('ref_axis',(1.,0.,0.));
#1781=DIRECTION('center_axis',(0.,-1.,0.));
#1782=DIRECTION('ref_axis',(1.,0.,0.));
#1783=DIRECTION('center_axis',(0.,-1.,0.));
#1784=DIRECTION('ref_axis',(1.,0.,0.));
#1785=DIRECTION('',(0.,-1.,0.));
#1786=DIRECTION('center_axis',(0.,1.,0.));
#1787=DIRECTION('ref_axis',(1.,0.,0.));
#1788=DIRECTION('center_axis',(0.,1.,0.));
#1789=DIRECTION('ref_axis',(1.,0.,0.));
#1790=DIRECTION('center_axis',(0.,1.,0.));
#1791=DIRECTION('ref_axis',(1.,0.,0.));
#1792=DIRECTION('',(0.,-1.,0.));
#1793=DIRECTION('center_axis',(0.,1.,0.));
#1794=DIRECTION('ref_axis',(1.,0.,0.));
#1795=DIRECTION('center_axis',(0.,1.,0.));
#1796=DIRECTION('ref_axis',(1.,0.,0.));
#1797=DIRECTION('center_axis',(0.,1.,0.));
#1798=DIRECTION('ref_axis',(1.,0.,0.));
#1799=DIRECTION('axis',(0.,0.,1.));
#1800=DIRECTION('refdir',(1.,0.,0.));
#1801=DIRECTION('center_axis',(0.,-1.,0.));
#1802=DIRECTION('ref_axis',(1.,0.,0.));
#1803=DIRECTION('center_axis',(0.,-1.,0.));
#1804=DIRECTION('ref_axis',(1.,0.,0.));
#1805=DIRECTION('center_axis',(0.,-1.,0.));
#1806=DIRECTION('ref_axis',(1.,0.,0.));
#1807=DIRECTION('',(0.,1.,0.));
#1808=DIRECTION('center_axis',(0.,-1.,0.));
#1809=DIRECTION('ref_axis',(1.,0.,0.));
#1810=DIRECTION('center_axis',(0.,1.,0.));
#1811=DIRECTION('ref_axis',(0.,0.,1.));
#1812=DIRECTION('axis',(0.,0.,1.));
#1813=DIRECTION('refdir',(1.,0.,0.));
#1814=DIRECTION('center_axis',(0.,-1.,0.));
#1815=DIRECTION('ref_axis',(1.,0.,0.));
#1816=DIRECTION('center_axis',(0.,-1.,0.));
#1817=DIRECTION('ref_axis',(1.,0.,0.));
#1818=DIRECTION('',(0.,-1.,0.));
#1819=DIRECTION('center_axis',(0.,1.,0.));
#1820=DIRECTION('ref_axis',(1.,0.,0.));
#1821=DIRECTION('center_axis',(0.,-1.,0.));
#1822=DIRECTION('ref_axis',(1.,0.,0.));
#1823=DIRECTION('center_axis',(0.,-1.,0.));
#1824=DIRECTION('ref_axis',(1.,0.,0.));
#1825=DIRECTION('',(0.,-1.,0.));
#1826=DIRECTION('center_axis',(0.,-1.,0.));
#1827=DIRECTION('ref_axis',(1.,0.,0.));
#1828=DIRECTION('center_axis',(0.,1.,0.));
#1829=DIRECTION('ref_axis',(0.,0.,1.));
#1830=DIRECTION('',(-1.,0.,0.));
#1831=DIRECTION('',(0.,0.,-1.));
#1832=DIRECTION('',(1.,0.,0.));
#1833=DIRECTION('',(0.,0.,1.));
#1834=DIRECTION('center_axis',(1.,0.,0.));
#1835=DIRECTION('ref_axis',(0.,0.,-1.));
#1836=DIRECTION('',(0.,1.,0.));
#1837=DIRECTION('',(0.,0.,-1.));
#1838=DIRECTION('',(0.,1.,0.));
#1839=DIRECTION('center_axis',(0.,0.,-1.));
#1840=DIRECTION('ref_axis',(-1.,0.,0.));
#1841=DIRECTION('',(0.,1.,0.));
#1842=DIRECTION('',(-1.,0.,0.));
#1843=DIRECTION('center_axis',(0.,0.,1.));
#1844=DIRECTION('ref_axis',(1.,0.,0.));
#1845=DIRECTION('',(1.,0.,0.));
#1846=DIRECTION('',(0.,1.,0.));
#1847=DIRECTION('center_axis',(-1.,0.,0.));
#1848=DIRECTION('ref_axis',(0.,0.,1.));
#1849=DIRECTION('',(0.,0.,1.));
#1850=DIRECTION('center_axis',(0.,1.,0.));
#1851=DIRECTION('ref_axis',(0.,0.,1.));
#1852=DIRECTION('',(0.,0.,1.));
#1853=DIRECTION('',(1.,0.,0.));
#1854=DIRECTION('',(0.,0.,1.));
#1855=DIRECTION('',(1.,0.,0.));
#1856=DIRECTION('',(0.,0.,1.));
#1857=DIRECTION('',(1.,0.,0.));
#1858=DIRECTION('',(0.,0.,1.));
#1859=DIRECTION('',(1.,0.,0.));
#1860=DIRECTION('',(0.,0.,1.));
#1861=DIRECTION('',(1.,0.,0.));
#1862=DIRECTION('',(0.,0.,1.));
#1863=DIRECTION('',(1.,0.,0.));
#1864=DIRECTION('',(0.,0.,1.));
#1865=DIRECTION('',(1.,0.,0.));
#1866=DIRECTION('',(0.,0.,1.));
#1867=DIRECTION('',(1.,0.,0.));
#1868=CARTESIAN_POINT('',(0.,0.,0.));
#1869=CARTESIAN_POINT('',(0.,0.,0.));
#1870=CARTESIAN_POINT('Origin',(0.,0.,64.2867316297599));
#1871=CARTESIAN_POINT('',(-2.5,0.,64.2867316297599));
#1872=CARTESIAN_POINT('Origin',(0.,0.,64.2867316297599));
#1873=CARTESIAN_POINT('',(-2.5,-5.,64.2867316297599));
#1874=CARTESIAN_POINT('',(-2.5,0.,64.2867316297599));
#1875=CARTESIAN_POINT('Origin',(0.,-5.,64.2867316297599));
#1876=CARTESIAN_POINT('Origin',(-34.7405684710615,0.,44.2292550711919));
#1877=CARTESIAN_POINT('',(-23.2587346574158,-5.,38.1327403065235));
#1878=CARTESIAN_POINT('',(-23.2587346574158,0.,38.1327403065235));
#1879=CARTESIAN_POINT('',(-23.2587346574158,0.,38.1327403065235));
#1880=CARTESIAN_POINT('',(-34.2793882249884,-5.,57.2210722181746));
#1881=CARTESIAN_POINT('Origin',(-34.7405684710615,-5.,44.2292550711919));
#1882=CARTESIAN_POINT('',(-34.2793882249884,0.,57.2210722181746));
#1883=CARTESIAN_POINT('',(-34.2793882249884,0.,57.2210722181746));
#1884=CARTESIAN_POINT('Origin',(-34.7405684710615,0.,44.2292550711919));
#1885=CARTESIAN_POINT('Origin',(-34.7405684710615,0.,84.3442081883279));
#1886=CARTESIAN_POINT('',(-34.2793882249884,-5.,71.3523910413453));
#1887=CARTESIAN_POINT('',(-34.2793882249884,0.,71.3523910413453));
#1888=CARTESIAN_POINT('',(-34.2793882249884,0.,71.3523910413453));
#1889=CARTESIAN_POINT('',(-23.2587346574157,-5.,90.4407229529964));
#1890=CARTESIAN_POINT('Origin',(-34.7405684710615,-5.,84.3442081883279));
#1891=CARTESIAN_POINT('',(-23.2587346574157,0.,90.4407229529964));
#1892=CARTESIAN_POINT('',(-23.2587346574157,0.,90.4407229529964));
#1893=CARTESIAN_POINT('Origin',(-34.7405684710615,0.,84.3442081883279));
#1894=CARTESIAN_POINT('Origin',(-8.88178419700125E-15,0.,104.401684746896));
#1895=CARTESIAN_POINT('',(-11.0206535675727,-5.,97.5063823645817));
#1896=CARTESIAN_POINT('',(-11.0206535675727,0.,97.5063823645817));
#1897=CARTESIAN_POINT('',(-11.0206535675727,0.,97.5063823645817));
#1898=CARTESIAN_POINT('',(11.0206535675727,-5.,97.5063823645817));
#1899=CARTESIAN_POINT('Origin',(-8.88178419700125E-15,-5.,104.401684746896));
#1900=CARTESIAN_POINT('',(11.0206535675727,0.,97.5063823645817));
#1901=CARTESIAN_POINT('',(11.0206535675727,0.,97.5063823645817));
#1902=CARTESIAN_POINT('Origin',(-8.88178419700125E-15,0.,104.401684746896));
#1903=CARTESIAN_POINT('Origin',(34.7405684710615,0.,84.3442081883279));
#1904=CARTESIAN_POINT('',(23.2587346574158,-5.,90.4407229529964));
#1905=CARTESIAN_POINT('',(23.2587346574158,0.,90.4407229529964));
#1906=CARTESIAN_POINT('',(23.2587346574158,0.,90.4407229529964));
#1907=CARTESIAN_POINT('',(34.2793882249884,-5.,71.3523910413453));
#1908=CARTESIAN_POINT('Origin',(34.7405684710615,-5.,84.3442081883279));
#1909=CARTESIAN_POINT('',(34.2793882249884,0.,71.3523910413453));
#1910=CARTESIAN_POINT('',(34.2793882249884,0.,71.3523910413453));
#1911=CARTESIAN_POINT('Origin',(34.7405684710615,0.,84.3442081883279));
#1912=CARTESIAN_POINT('Origin',(34.7405684710615,0.,44.2292550711919));
#1913=CARTESIAN_POINT('',(34.2793882249884,-5.,57.2210722181745));
#1914=CARTESIAN_POINT('',(34.2793882249884,0.,57.2210722181745));
#1915=CARTESIAN_POINT('',(34.2793882249884,0.,57.2210722181745));
#1916=CARTESIAN_POINT('',(23.2587346574157,-5.,38.1327403065234));
#1917=CARTESIAN_POINT('Origin',(34.7405684710615,-5.,44.2292550711919));
#1918=CARTESIAN_POINT('',(23.2587346574157,0.,38.1327403065234));
#1919=CARTESIAN_POINT('',(23.2587346574157,0.,38.1327403065234));
#1920=CARTESIAN_POINT('Origin',(34.7405684710615,0.,44.2292550711919));
#1921=CARTESIAN_POINT('Origin',(0.,0.,64.2867316297599));
#1922=CARTESIAN_POINT('',(-34.9106001094224,-5.,61.7867316297599));
#1923=CARTESIAN_POINT('Origin',(0.,-5.,64.2867316297599));
#1924=CARTESIAN_POINT('',(-34.9106001094224,0.,61.7867316297599));
#1925=CARTESIAN_POINT('',(-34.9106001094224,0.,61.7867316297599));
#1926=CARTESIAN_POINT('Origin',(0.,0.,64.2867316297599));
#1927=CARTESIAN_POINT('Origin',(0.,0.,64.2867316297599));
#1928=CARTESIAN_POINT('',(-19.6203635641723,-5.,93.2701981858795));
#1929=CARTESIAN_POINT('Origin',(0.,-5.,64.2867316297599));
#1930=CARTESIAN_POINT('',(-19.6203635641723,0.,93.2701981858795));
#1931=CARTESIAN_POINT('',(-19.6203635641723,0.,93.2701981858795));
#1932=CARTESIAN_POINT('Origin',(0.,0.,64.2867316297599));
#1933=CARTESIAN_POINT('Origin',(0.,0.,64.2867316297599));
#1934=CARTESIAN_POINT('',(15.2902365452501,-5.,95.7701981858795));
#1935=CARTESIAN_POINT('Origin',(0.,-5.,64.2867316297599));
#1936=CARTESIAN_POINT('',(15.2902365452501,0.,95.7701981858795));
#1937=CARTESIAN_POINT('',(15.2902365452501,0.,95.7701981858795));
#1938=CARTESIAN_POINT('Origin',(0.,0.,64.2867316297599));
#1939=CARTESIAN_POINT('Origin',(0.,0.,64.2867316297599));
#1940=CARTESIAN_POINT('',(34.9106001094224,-5.,66.7867316297599));
#1941=CARTESIAN_POINT('Origin',(0.,-5.,64.2867316297599));
#1942=CARTESIAN_POINT('',(34.9106001094224,0.,66.7867316297599));
#1943=CARTESIAN_POINT('',(34.9106001094224,0.,66.7867316297599));
#1944=CARTESIAN_POINT('Origin',(0.,0.,64.2867316297599));
#1945=CARTESIAN_POINT('Origin',(17.4553000547112,0.,81.7867316297599));
#1946=CARTESIAN_POINT('',(-13.316088815901,0.,61.7867316297599));
#1947=CARTESIAN_POINT('',(-13.316088815901,0.,61.7867316297599));
#1948=CARTESIAN_POINT('',(-13.316088815901,0.,66.7867316297599));
#1949=CARTESIAN_POINT('Origin',(-13.316088815901,0.,64.2867316297599));
#1950=CARTESIAN_POINT('',(-34.9106001094224,0.,66.7867316297599));
#1951=CARTESIAN_POINT('',(-13.316088815901,0.,66.7867316297599));
#1952=CARTESIAN_POINT('Origin',(0.,0.,64.2867316297599));
#1953=CARTESIAN_POINT('',(-8.82310791741161,0.,74.56880282338));
#1954=CARTESIAN_POINT('',(-22.4951260134151,0.,98.2494328076592));
#1955=CARTESIAN_POINT('',(-4.49298089848941,0.,77.06880282338));
#1956=CARTESIAN_POINT('Origin',(-6.65804440795051,0.,75.81880282338));
#1957=CARTESIAN_POINT('',(-15.2902365452501,0.,95.7701981858795));
#1958=CARTESIAN_POINT('',(-4.49298089848941,0.,77.06880282338));
#1959=CARTESIAN_POINT('Origin',(0.,0.,64.2867316297599));
#1960=CARTESIAN_POINT('',(4.49298089848941,0.,77.06880282338));
#1961=CARTESIAN_POINT('',(4.49298089848941,0.,77.06880282338));
#1962=CARTESIAN_POINT('',(8.82310791741161,0.,74.56880282338));
#1963=CARTESIAN_POINT('Origin',(6.65804440795051,0.,75.81880282338));
#1964=CARTESIAN_POINT('',(19.6203635641723,0.,93.2701981858795));
#1965=CARTESIAN_POINT('',(22.4951260134151,0.,98.2494328076592));
#1966=CARTESIAN_POINT('Origin',(0.,0.,64.2867316297599));
#1967=CARTESIAN_POINT('',(13.316088815901,0.,66.7867316297599));
#1968=CARTESIAN_POINT('',(13.316088815901,0.,66.7867316297599));
#1969=CARTESIAN_POINT('',(13.316088815901,0.,61.7867316297599));
#1970=CARTESIAN_POINT('Origin',(13.316088815901,0.,64.2867316297599));
#1971=CARTESIAN_POINT('',(34.9106001094224,0.,61.7867316297599));
#1972=CARTESIAN_POINT('',(13.316088815901,0.,61.7867316297599));
#1973=CARTESIAN_POINT('Origin',(0.,0.,64.2867316297599));
#1974=CARTESIAN_POINT('',(19.6203635641723,0.,35.3032650736403));
#1975=CARTESIAN_POINT('Origin',(0.,0.,64.2867316297599));
#1976=CARTESIAN_POINT('',(8.82310791741161,0.,54.0046604361398));
#1977=CARTESIAN_POINT('',(22.4951260134151,0.,30.3240304518606));
#1978=CARTESIAN_POINT('',(4.49298089848941,0.,51.5046604361398));
#1979=CARTESIAN_POINT('Origin',(6.65804440795051,0.,52.7546604361398));
#1980=CARTESIAN_POINT('',(15.2902365452501,0.,32.8032650736403));
#1981=CARTESIAN_POINT('',(4.49298089848941,0.,51.5046604361398));
#1982=CARTESIAN_POINT('',(11.0206535675727,0.,31.0670808949381));
#1983=CARTESIAN_POINT('Origin',(0.,0.,64.2867316297599));
#1984=CARTESIAN_POINT('',(-11.0206535675727,0.,31.0670808949381));
#1985=CARTESIAN_POINT('Origin',(0.,0.,24.1717785126239));
#1986=CARTESIAN_POINT('',(-15.2902365452501,0.,32.8032650736403));
#1987=CARTESIAN_POINT('Origin',(0.,0.,64.2867316297599));
#1988=CARTESIAN_POINT('',(-4.49298089848941,0.,51.5046604361398));
#1989=CARTESIAN_POINT('',(-4.49298089848941,0.,51.5046604361398));
#1990=CARTESIAN_POINT('',(-8.82310791741161,0.,54.0046604361398));
#1991=CARTESIAN_POINT('Origin',(-6.65804440795051,0.,52.7546604361398));
#1992=CARTESIAN_POINT('',(-19.6203635641723,0.,35.3032650736403));
#1993=CARTESIAN_POINT('',(-22.4951260134151,0.,30.3240304518606));
#1994=CARTESIAN_POINT('Origin',(0.,0.,64.2867316297599));
#1995=CARTESIAN_POINT('Origin',(0.,0.,64.2867316297599));
#1996=CARTESIAN_POINT('',(19.6203635641723,-5.,35.3032650736403));
#1997=CARTESIAN_POINT('Origin',(0.,-5.,64.2867316297599));
#1998=CARTESIAN_POINT('',(19.6203635641723,0.,35.3032650736403));
#1999=CARTESIAN_POINT('Origin',(0.,0.,24.1717785126239));
#2000=CARTESIAN_POINT('',(-11.0206535675727,-5.,31.0670808949381));
#2001=CARTESIAN_POINT('',(-11.0206535675727,0.,31.0670808949381));
#2002=CARTESIAN_POINT('',(11.0206535675727,-5.,31.0670808949381));
#2003=CARTESIAN_POINT('',(11.0206535675727,0.,31.0670808949381));
#2004=CARTESIAN_POINT('Origin',(0.,-5.,24.1717785126239));
#2005=CARTESIAN_POINT('Origin',(17.4553000547112,-5.,81.7867316297599));
#2006=CARTESIAN_POINT('',(-19.6203635641723,-5.,35.3032650736403));
#2007=CARTESIAN_POINT('Origin',(0.,-5.,64.2867316297599));
#2008=CARTESIAN_POINT('',(-8.82310791741161,-5.,54.0046604361398));
#2009=CARTESIAN_POINT('',(-22.4951260134151,-5.,30.3240304518606));
#2010=CARTESIAN_POINT('',(-4.49298089848941,-5.,51.5046604361398));
#2011=CARTESIAN_POINT('Origin',(-6.65804440795051,-5.,52.7546604361398));
#2012=CARTESIAN_POINT('',(-15.2902365452501,-5.,32.8032650736403));
#2013=CARTESIAN_POINT('',(-4.49298089848941,-5.,51.5046604361398));
#2014=CARTESIAN_POINT('Origin',(0.,-5.,64.2867316297599));
#2015=CARTESIAN_POINT('',(15.2902365452501,-5.,32.8032650736403));
#2016=CARTESIAN_POINT('Origin',(0.,-5.,64.2867316297599));
#2017=CARTESIAN_POINT('',(4.49298089848941,-5.,51.5046604361398));
#2018=CARTESIAN_POINT('',(4.49298089848941,-5.,51.5046604361398));
#2019=CARTESIAN_POINT('',(8.82310791741161,-5.,54.0046604361398));
#2020=CARTESIAN_POINT('Origin',(6.65804440795051,-5.,52.7546604361398));
#2021=CARTESIAN_POINT('',(22.4951260134151,-5.,30.3240304518606));
#2022=CARTESIAN_POINT('',(34.9106001094224,-5.,61.7867316297599));
#2023=CARTESIAN_POINT('Origin',(0.,-5.,64.2867316297599));
#2024=CARTESIAN_POINT('',(13.316088815901,-5.,61.7867316297599));
#2025=CARTESIAN_POINT('',(13.316088815901,-5.,61.7867316297599));
#2026=CARTESIAN_POINT('',(13.316088815901,-5.,66.7867316297599));
#2027=CARTESIAN_POINT('Origin',(13.316088815901,-5.,64.2867316297599));
#2028=CARTESIAN_POINT('',(13.316088815901,-5.,66.7867316297599));
#2029=CARTESIAN_POINT('',(19.6203635641723,-5.,93.2701981858795));
#2030=CARTESIAN_POINT('Origin',(0.,-5.,64.2867316297599));
#2031=CARTESIAN_POINT('',(8.82310791741161,-5.,74.56880282338));
#2032=CARTESIAN_POINT('',(22.4951260134151,-5.,98.2494328076592));
#2033=CARTESIAN_POINT('',(4.49298089848941,-5.,77.06880282338));
#2034=CARTESIAN_POINT('Origin',(6.65804440795051,-5.,75.81880282338));
#2035=CARTESIAN_POINT('',(4.49298089848941,-5.,77.06880282338));
#2036=CARTESIAN_POINT('',(-15.2902365452501,-5.,95.7701981858795));
#2037=CARTESIAN_POINT('Origin',(0.,-5.,64.2867316297599));
#2038=CARTESIAN_POINT('',(-4.49298089848941,-5.,77.06880282338));
#2039=CARTESIAN_POINT('',(-4.49298089848941,-5.,77.06880282338));
#2040=CARTESIAN_POINT('',(-8.82310791741161,-5.,74.56880282338));
#2041=CARTESIAN_POINT('Origin',(-6.65804440795051,-5.,75.81880282338));
#2042=CARTESIAN_POINT('',(-22.4951260134151,-5.,98.2494328076592));
#2043=CARTESIAN_POINT('',(-34.9106001094224,-5.,66.7867316297599));
#2044=CARTESIAN_POINT('Origin',(0.,-5.,64.2867316297599));
#2045=CARTESIAN_POINT('',(-13.316088815901,-5.,66.7867316297599));
#2046=CARTESIAN_POINT('',(-13.316088815901,-5.,66.7867316297599));
#2047=CARTESIAN_POINT('',(-13.316088815901,-5.,61.7867316297599));
#2048=CARTESIAN_POINT('Origin',(-13.316088815901,-5.,64.2867316297599));
#2049=CARTESIAN_POINT('',(-13.316088815901,-5.,61.7867316297599));
#2050=CARTESIAN_POINT('Origin',(0.,0.,64.2867316297599));
#2051=CARTESIAN_POINT('',(15.2902365452501,0.,32.8032650736403));
#2052=CARTESIAN_POINT('Origin',(0.,0.,64.2867316297599));
#2053=CARTESIAN_POINT('',(-15.2902365452501,0.,32.8032650736403));
#2054=CARTESIAN_POINT('Origin',(-4.49298089848941,0.,51.5046604361398));
#2055=CARTESIAN_POINT('',(-4.49298089848941,0.,51.5046604361398));
#2056=CARTESIAN_POINT('Origin',(-6.65804440795051,0.,52.7546604361398));
#2057=CARTESIAN_POINT('',(-8.82310791741161,0.,54.0046604361398));
#2058=CARTESIAN_POINT('Origin',(-19.6203635641723,0.,35.3032650736403));
#2059=CARTESIAN_POINT('',(-19.6203635641723,0.,35.3032650736403));
#2060=CARTESIAN_POINT('Origin',(0.,0.,64.2867316297599));
#2061=CARTESIAN_POINT('Origin',(-13.316088815901,0.,61.7867316297599));
#2062=CARTESIAN_POINT('',(-13.316088815901,0.,61.7867316297599));
#2063=CARTESIAN_POINT('Origin',(4.49298089848941,0.,51.5046604361398));
#2064=CARTESIAN_POINT('',(4.49298089848941,0.,51.5046604361398));
#2065=CARTESIAN_POINT('Origin',(6.65804440795051,0.,52.7546604361398));
#2066=CARTESIAN_POINT('',(8.82310791741161,0.,54.0046604361398));
#2067=CARTESIAN_POINT('Origin',(19.6203635641723,0.,35.3032650736403));
#2068=CARTESIAN_POINT('Origin',(0.,0.,64.2867316297599));
#2069=CARTESIAN_POINT('',(34.9106001094224,0.,61.7867316297599));
#2070=CARTESIAN_POINT('Origin',(13.316088815901,0.,61.7867316297599));
#2071=CARTESIAN_POINT('',(13.316088815901,0.,61.7867316297599));
#2072=CARTESIAN_POINT('Origin',(-4.49298089848941,0.,77.06880282338));
#2073=CARTESIAN_POINT('',(-4.49298089848941,0.,77.06880282338));
#2074=CARTESIAN_POINT('',(-15.2902365452501,0.,95.7701981858795));
#2075=CARTESIAN_POINT('Origin',(-6.65804440795051,0.,75.81880282338));
#2076=CARTESIAN_POINT('',(-8.82310791741161,0.,74.56880282338));
#2077=CARTESIAN_POINT('Origin',(-19.6203635641723,0.,93.2701981858795));
#2078=CARTESIAN_POINT('Origin',(0.,0.,64.2867316297599));
#2079=CARTESIAN_POINT('',(-34.9106001094224,0.,66.7867316297599));
#2080=CARTESIAN_POINT('Origin',(-13.316088815901,0.,66.7867316297599));
#2081=CARTESIAN_POINT('',(-13.316088815901,0.,66.7867316297599));
#2082=CARTESIAN_POINT('Origin',(-13.316088815901,0.,64.2867316297599));
#2083=CARTESIAN_POINT('Origin',(0.,0.,64.2867316297599));
#2084=CARTESIAN_POINT('Origin',(4.49298089848941,0.,77.06880282338));
#2085=CARTESIAN_POINT('',(4.49298089848941,0.,77.06880282338));
#2086=CARTESIAN_POINT('Origin',(6.65804440795051,0.,75.81880282338));
#2087=CARTESIAN_POINT('',(8.82310791741161,0.,74.56880282338));
#2088=CARTESIAN_POINT('Origin',(19.6203635641723,0.,93.2701981858795));
#2089=CARTESIAN_POINT('',(19.6203635641723,0.,93.2701981858795));
#2090=CARTESIAN_POINT('Origin',(0.,0.,64.2867316297599));
#2091=CARTESIAN_POINT('Origin',(13.316088815901,0.,66.7867316297599));
#2092=CARTESIAN_POINT('',(13.316088815901,0.,66.7867316297599));
#2093=CARTESIAN_POINT('Origin',(13.316088815901,0.,64.2867316297599));
#2094=CARTESIAN_POINT('',(0.,0.,0.));
#2095=CARTESIAN_POINT('Origin',(-17.3702842355308,-5.,34.2005167919079));
#2096=CARTESIAN_POINT('',(-19.6202842355308,-5.,34.2005167919079));
#2097=CARTESIAN_POINT('Origin',(-17.3702842355308,-5.,34.2005167919079));
#2098=CARTESIAN_POINT('Origin',(-17.3702842355308,0.,34.2005167919079));
#2099=CARTESIAN_POINT('',(-19.6202842355308,3.,34.2005167919079));
#2100=CARTESIAN_POINT('',(-19.6202842355308,0.,34.2005167919079));
#2101=CARTESIAN_POINT('Origin',(-17.3702842355308,3.,34.2005167919079));
#2102=CARTESIAN_POINT('Origin',(0.,3.,24.1717785126239));
#2103=CARTESIAN_POINT('',(0.,0.,0.));
#2104=CARTESIAN_POINT('Origin',(0.,-5.,64.2867316297599));
#2105=CARTESIAN_POINT('',(-2.5,-5.,64.2867316297599));
#2106=CARTESIAN_POINT('Origin',(0.,-5.,64.2867316297599));
#2107=CARTESIAN_POINT('Origin',(0.,3.,64.2867316297599));
#2108=CARTESIAN_POINT('',(-2.5,5.,64.2867316297599));
#2109=CARTESIAN_POINT('',(-2.5,3.,64.2867316297599));
#2110=CARTESIAN_POINT('Origin',(0.,5.,64.2867316297599));
#2111=CARTESIAN_POINT('Origin',(0.,5.,50.));
#2112=CARTESIAN_POINT('',(0.,0.,0.));
#2113=CARTESIAN_POINT('Origin',(0.,0.,24.1717785126239));
#2114=CARTESIAN_POINT('',(-2.5,3.,24.1717785126239));
#2115=CARTESIAN_POINT('Origin',(0.,3.,24.1717785126239));
#2116=CARTESIAN_POINT('',(-2.5,-5.,24.1717785126239));
#2117=CARTESIAN_POINT('',(-2.5,0.,24.1717785126239));
#2118=CARTESIAN_POINT('Origin',(0.,-5.,24.1717785126239));
#2119=CARTESIAN_POINT('Origin',(0.,-5.,24.1717785126239));
#2120=CARTESIAN_POINT('',(-13.,-5.,24.1717785126239));
#2121=CARTESIAN_POINT('Origin',(0.,-5.,24.1717785126239));
#2122=CARTESIAN_POINT('Origin',(0.,0.,24.1717785126239));
#2123=CARTESIAN_POINT('',(-13.,3.,24.1717785126239));
#2124=CARTESIAN_POINT('',(-13.,0.,24.1717785126239));
#2125=CARTESIAN_POINT('Origin',(0.,3.,24.1717785126239));
#2126=CARTESIAN_POINT('Origin',(0.,3.,24.1717785126239));
#2127=CARTESIAN_POINT('',(0.,0.,0.));
#2128=CARTESIAN_POINT('Origin',(0.,0.,64.2867316297599));
#2129=CARTESIAN_POINT('',(-4.5,0.,64.2867316297599));
#2130=CARTESIAN_POINT('Origin',(0.,0.,64.2867316297599));
#2131=CARTESIAN_POINT('',(-2.5,0.,64.2867316297599));
#2132=CARTESIAN_POINT('Origin',(0.,0.,64.2867316297599));
#2133=CARTESIAN_POINT('Origin',(0.,3.,64.2867316297599));
#2134=CARTESIAN_POINT('',(-4.5,3.,64.2867316297599));
#2135=CARTESIAN_POINT('',(-4.5,3.,64.2867316297599));
#2136=CARTESIAN_POINT('Origin',(0.,3.,64.2867316297599));
#2137=CARTESIAN_POINT('Origin',(0.,3.,64.2867316297599));
#2138=CARTESIAN_POINT('',(-2.5,3.,64.2867316297599));
#2139=CARTESIAN_POINT('Origin',(0.,3.,64.2867316297599));
#2140=CARTESIAN_POINT('',(-2.5,3.,64.2867316297599));
#2141=CARTESIAN_POINT('Origin',(0.,3.,50.));
#2142=CARTESIAN_POINT('',(0.,0.,0.));
#2143=CARTESIAN_POINT('Origin',(0.,0.,24.1717785126239));
#2144=CARTESIAN_POINT('',(-13.,3.,24.1717785126239));
#2145=CARTESIAN_POINT('Origin',(0.,3.,24.1717785126239));
#2146=CARTESIAN_POINT('',(-13.,0.,24.1717785126239));
#2147=CARTESIAN_POINT('',(-13.,0.,24.1717785126239));
#2148=CARTESIAN_POINT('Origin',(0.,0.,24.1717785126239));
#2149=CARTESIAN_POINT('Origin',(-17.3702842355308,0.,34.2005167919079));
#2150=CARTESIAN_POINT('',(-19.6202842355308,3.,34.2005167919079));
#2151=CARTESIAN_POINT('Origin',(-17.3702842355308,3.,34.2005167919079));
#2152=CARTESIAN_POINT('',(-19.6202842355308,0.,34.2005167919079));
#2153=CARTESIAN_POINT('',(-19.6202842355308,0.,34.2005167919079));
#2154=CARTESIAN_POINT('Origin',(-17.3702842355308,0.,34.2005167919079));
#2155=CARTESIAN_POINT('Origin',(0.,0.,24.1717785126239));
#2156=CARTESIAN_POINT('',(-24.1717785126239,3.,24.1717785126239));
#2157=CARTESIAN_POINT('Origin',(0.,3.,24.1717785126239));
#2158=CARTESIAN_POINT('',(-24.1717785126239,0.,24.1717785126239));
#2159=CARTESIAN_POINT('',(-24.1717785126239,0.,24.1717785126239));
#2160=CARTESIAN_POINT('Origin',(0.,0.,24.1717785126239));
#2161=CARTESIAN_POINT('Origin',(0.,3.,24.1717785126239));
#2162=CARTESIAN_POINT('Origin',(0.,0.,24.1717785126239));
#2163=CARTESIAN_POINT('',(0.,0.,0.));
#2164=CARTESIAN_POINT('Origin',(0.,-5.,24.1717785126239));
#2165=CARTESIAN_POINT('',(-2.5,-5.,24.1717785126239));
#2166=CARTESIAN_POINT('Origin',(0.,-5.,24.1717785126239));
#2167=CARTESIAN_POINT('Origin',(0.,3.,24.1717785126239));
#2168=CARTESIAN_POINT('',(-2.5,5.,24.1717785126239));
#2169=CARTESIAN_POINT('',(-2.5,3.,24.1717785126239));
#2170=CARTESIAN_POINT('Origin',(0.,5.,24.1717785126239));
#2171=CARTESIAN_POINT('Origin',(0.,5.,50.));
#2172=CARTESIAN_POINT('',(0.,0.,0.));
#2173=CARTESIAN_POINT('Origin',(0.,3.,24.1717785126239));
#2174=CARTESIAN_POINT('',(-2.5,5.,24.1717785126239));
#2175=CARTESIAN_POINT('Origin',(0.,5.,24.1717785126239));
#2176=CARTESIAN_POINT('',(-2.5,3.,24.1717785126239));
#2177=CARTESIAN_POINT('',(-2.5,3.,24.1717785126239));
#2178=CARTESIAN_POINT('Origin',(0.,3.,24.1717785126239));
#2179=CARTESIAN_POINT('Origin',(0.,3.,64.2867316297599));
#2180=CARTESIAN_POINT('',(-2.5,5.,64.2867316297599));
#2181=CARTESIAN_POINT('Origin',(0.,5.,64.2867316297599));
#2182=CARTESIAN_POINT('',(-2.5,3.,64.2867316297599));
#2183=CARTESIAN_POINT('',(-2.5,3.,64.2867316297599));
#2184=CARTESIAN_POINT('Origin',(0.,3.,64.2867316297599));
#2185=CARTESIAN_POINT('Origin',(0.,3.,50.));
#2186=CARTESIAN_POINT('',(39.8793542860875,3.,-5.));
#2187=CARTESIAN_POINT('',(-39.8793542860875,3.,-5.));
#2188=CARTESIAN_POINT('',(19.9396771430438,3.,-5.));
#2189=CARTESIAN_POINT('',(39.8793542860875,3.,105.));
#2190=CARTESIAN_POINT('',(39.8793542860875,3.,77.5));
#2191=CARTESIAN_POINT('',(-39.8793542860875,3.,105.));
#2192=CARTESIAN_POINT('',(-19.9396771430438,3.,105.));
#2193=CARTESIAN_POINT('',(-39.8793542860875,3.,22.5));
#2194=CARTESIAN_POINT('Origin',(39.8793542860875,0.,105.));
#2195=CARTESIAN_POINT('',(39.8793542860875,5.,-5.));
#2196=CARTESIAN_POINT('',(39.8793542860875,0.,-5.));
#2197=CARTESIAN_POINT('',(39.8793542860875,5.,105.));
#2198=CARTESIAN_POINT('',(39.8793542860875,5.,105.));
#2199=CARTESIAN_POINT('',(39.8793542860875,0.,105.));
#2200=CARTESIAN_POINT('Origin',(39.8793542860875,0.,-5.));
#2201=CARTESIAN_POINT('',(-39.8793542860875,5.,-5.));
#2202=CARTESIAN_POINT('',(-39.8793542860875,0.,-5.));
#2203=CARTESIAN_POINT('',(39.8793542860875,5.,-5.));
#2204=CARTESIAN_POINT('Origin',(-39.8793542860875,0.,105.));
#2205=CARTESIAN_POINT('',(-39.8793542860875,5.,105.));
#2206=CARTESIAN_POINT('',(-39.8793542860875,5.,105.));
#2207=CARTESIAN_POINT('',(-39.8793542860875,0.,105.));
#2208=CARTESIAN_POINT('Origin',(-39.8793542860875,0.,-5.));
#2209=CARTESIAN_POINT('',(-39.8793542860875,5.,-5.));
#2210=CARTESIAN_POINT('Origin',(0.,5.,50.));
#2211=CARTESIAN_POINT('',(0.,0.,0.));
#2212=CARTESIAN_POINT('',(0.,0.,0.));
#2213=CARTESIAN_POINT('',(0.,0.,0.));
#2214=CARTESIAN_POINT('',(0.,0.,0.));
#2215=CARTESIAN_POINT('',(0.,0.,0.));
#2216=CARTESIAN_POINT('',(0.,0.,0.));
#2217=CARTESIAN_POINT('',(0.,0.,0.));
#2218=CARTESIAN_POINT('',(0.,0.,0.));
#2219=UNCERTAINTY_MEASURE_WITH_UNIT(LENGTH_MEASURE(0.01),#2239,
'DISTANCE_ACCURACY_VALUE',
'Maximum model space distance between geometric entities at asserted c
onnectivities');
#2220=UNCERTAINTY_MEASURE_WITH_UNIT(LENGTH_MEASURE(0.01),#2239,
'DISTANCE_ACCURACY_VALUE',
'Maximum model space distance between geometric entities at asserted c
onnectivities');
#2221=UNCERTAINTY_MEASURE_WITH_UNIT(LENGTH_MEASURE(0.01),#2239,
'DISTANCE_ACCURACY_VALUE',
'Maximum model space distance between geometric entities at asserted c
onnectivities');
#2222=UNCERTAINTY_MEASURE_WITH_UNIT(LENGTH_MEASURE(0.01),#2239,
'DISTANCE_ACCURACY_VALUE',
'Maximum model space distance between geometric entities at asserted c
onnectivities');
#2223=UNCERTAINTY_MEASURE_WITH_UNIT(LENGTH_MEASURE(0.01),#2239,
'DISTANCE_ACCURACY_VALUE',
'Maximum model space distance between geometric entities at asserted c
onnectivities');
#2224=UNCERTAINTY_MEASURE_WITH_UNIT(LENGTH_MEASURE(0.01),#2239,
'DISTANCE_ACCURACY_VALUE',
'Maximum model space distance between geometric entities at asserted c
onnectivities');
#2225=UNCERTAINTY_MEASURE_WITH_UNIT(LENGTH_MEASURE(0.01),#2239,
'DISTANCE_ACCURACY_VALUE',
'Maximum model space distance between geometric entities at asserted c
onnectivities');
#2226=UNCERTAINTY_MEASURE_WITH_UNIT(LENGTH_MEASURE(0.01),#2239,
'DISTANCE_ACCURACY_VALUE',
'Maximum model space distance between geometric entities at asserted c
onnectivities');
#2227=UNCERTAINTY_MEASURE_WITH_UNIT(LENGTH_MEASURE(0.01),#2239,
'DISTANCE_ACCURACY_VALUE',
'Maximum model space distance between geometric entities at asserted c
onnectivities');
#2228=UNCERTAINTY_MEASURE_WITH_UNIT(LENGTH_MEASURE(0.01),#2239,
'DISTANCE_ACCURACY_VALUE',
'Maximum model space distance between geometric entities at asserted c
onnectivities');
#2229=(
GEOMETRIC_REPRESENTATION_CONTEXT(3)
GLOBAL_UNCERTAINTY_ASSIGNED_CONTEXT((#2219))
GLOBAL_UNIT_ASSIGNED_CONTEXT((#2239,#2241,#2242))
REPRESENTATION_CONTEXT('','3D')
);
#2230=(
GEOMETRIC_REPRESENTATION_CONTEXT(3)
GLOBAL_UNCERTAINTY_ASSIGNED_CONTEXT((#2220))
GLOBAL_UNIT_ASSIGNED_CONTEXT((#2239,#2241,#2242))
REPRESENTATION_CONTEXT('','3D')
);
#2231=(
GEOMETRIC_REPRESENTATION_CONTEXT(3)
GLOBAL_UNCERTAINTY_ASSIGNED_CONTEXT((#2221))
GLOBAL_UNIT_ASSIGNED_CONTEXT((#2239,#2241,#2242))
REPRESENTATION_CONTEXT('','3D')
);
#2232=(
GEOMETRIC_REPRESENTATION_CONTEXT(3)
GLOBAL_UNCERTAINTY_ASSIGNED_CONTEXT((#2222))
GLOBAL_UNIT_ASSIGNED_CONTEXT((#2239,#2241,#2242))
REPRESENTATION_CONTEXT('','3D')
);
#2233=(
GEOMETRIC_REPRESENTATION_CONTEXT(3)
GLOBAL_UNCERTAINTY_ASSIGNED_CONTEXT((#2223))
GLOBAL_UNIT_ASSIGNED_CONTEXT((#2239,#2241,#2242))
REPRESENTATION_CONTEXT('','3D')
);
#2234=(
GEOMETRIC_REPRESENTATION_CONTEXT(3)
GLOBAL_UNCERTAINTY_ASSIGNED_CONTEXT((#2224))
GLOBAL_UNIT_ASSIGNED_CONTEXT((#2239,#2241,#2242))
REPRESENTATION_CONTEXT('','3D')
);
#2235=(
GEOMETRIC_REPRESENTATION_CONTEXT(3)
GLOBAL_UNCERTAINTY_ASSIGNED_CONTEXT((#2225))
GLOBAL_UNIT_ASSIGNED_CONTEXT((#2239,#2241,#2242))
REPRESENTATION_CONTEXT('','3D')
);
#2236=(
GEOMETRIC_REPRESENTATION_CONTEXT(3)
GLOBAL_UNCERTAINTY_ASSIGNED_CONTEXT((#2226))
GLOBAL_UNIT_ASSIGNED_CONTEXT((#2239,#2241,#2242))
REPRESENTATION_CONTEXT('','3D')
);
#2237=(
GEOMETRIC_REPRESENTATION_CONTEXT(3)
GLOBAL_UNCERTAINTY_ASSIGNED_CONTEXT((#2227))
GLOBAL_UNIT_ASSIGNED_CONTEXT((#2239,#2241,#2242))
REPRESENTATION_CONTEXT('','3D')
);
#2238=(
GEOMETRIC_REPRESENTATION_CONTEXT(3)
GLOBAL_UNCERTAINTY_ASSIGNED_CONTEXT((#2228))
GLOBAL_UNIT_ASSIGNED_CONTEXT((#2239,#2241,#2242))
REPRESENTATION_CONTEXT('','3D')
);
#2239=(
LENGTH_UNIT()
NAMED_UNIT(*)
SI_UNIT(.MILLI.,.METRE.)
);
#2240=(
LENGTH_UNIT()
NAMED_UNIT(*)
SI_UNIT($,.METRE.)
);
#2241=(
NAMED_UNIT(*)
PLANE_ANGLE_UNIT()
SI_UNIT($,.RADIAN.)
);
#2242=(
NAMED_UNIT(*)
SI_UNIT($,.STERADIAN.)
SOLID_ANGLE_UNIT()
);
#2243=SHAPE_DEFINITION_REPRESENTATION(#2252,#2269);
#2244=SHAPE_DEFINITION_REPRESENTATION(#2253,#2270);
#2245=SHAPE_DEFINITION_REPRESENTATION(#2254,#2271);
#2246=SHAPE_DEFINITION_REPRESENTATION(#2255,#2272);
#2247=SHAPE_DEFINITION_REPRESENTATION(#2256,#2273);
#2248=SHAPE_DEFINITION_REPRESENTATION(#2257,#2274);
#2249=SHAPE_DEFINITION_REPRESENTATION(#2258,#2275);
#2250=SHAPE_DEFINITION_REPRESENTATION(#2259,#2276);
#2251=SHAPE_DEFINITION_REPRESENTATION(#2260,#2277);
#2252=PRODUCT_DEFINITION_SHAPE('',$,#2279);
#2253=PRODUCT_DEFINITION_SHAPE('',$,#2280);
#2254=PRODUCT_DEFINITION_SHAPE('',$,#2281);
#2255=PRODUCT_DEFINITION_SHAPE('',$,#2282);
#2256=PRODUCT_DEFINITION_SHAPE('',$,#2283);
#2257=PRODUCT_DEFINITION_SHAPE('',$,#2284);
#2258=PRODUCT_DEFINITION_SHAPE('',$,#2285);
#2259=PRODUCT_DEFINITION_SHAPE('',$,#2286);
#2260=PRODUCT_DEFINITION_SHAPE('',$,#2287);
#2261=PRODUCT_DEFINITION_SHAPE($,$,#35);
#2262=PRODUCT_DEFINITION_SHAPE($,$,#36);
#2263=PRODUCT_DEFINITION_SHAPE($,$,#37);
#2264=PRODUCT_DEFINITION_SHAPE($,$,#38);
#2265=PRODUCT_DEFINITION_SHAPE($,$,#39);
#2266=PRODUCT_DEFINITION_SHAPE($,$,#40);
#2267=PRODUCT_DEFINITION_SHAPE($,$,#41);
#2268=PRODUCT_DEFINITION_SHAPE($,$,#42);
#2269=SHAPE_REPRESENTATION('',(#1303,#1455,#1456,#1457,#1458,#1459,#1460,
#1461,#1462),#2229);
#2270=SHAPE_REPRESENTATION('',(#1304),#2230);
#2271=SHAPE_REPRESENTATION('',(#1394),#2231);
#2272=SHAPE_REPRESENTATION('',(#1400),#2232);
#2273=SHAPE_REPRESENTATION('',(#1406),#2233);
#2274=SHAPE_REPRESENTATION('',(#1415),#2234);
#2275=SHAPE_REPRESENTATION('',(#1424),#2235);
#2276=SHAPE_REPRESENTATION('',(#1436),#2236);
#2277=SHAPE_REPRESENTATION('',(#1442),#2237);
#2278=PRODUCT_DEFINITION_CONTEXT('part definition',#2307,'design');
#2279=PRODUCT_DEFINITION('BR-052','BR-052',#2288,#2278);
#2280=PRODUCT_DEFINITION('Wheel','Wheel',#2289,#2278);
#2281=PRODUCT_DEFINITION('Pin_01','Pin_01',#2290,#2278);
#2282=PRODUCT_DEFINITION('Pin_02','Pin_02',#2291,#2278);
#2283=PRODUCT_DEFINITION('Crank_01','Crank_01',#2292,#2278);
#2284=PRODUCT_DEFINITION('Spacer','Spacer',#2293,#2278);
#2285=PRODUCT_DEFINITION('Crank_02','Crank_02',#2294,#2278);
#2286=PRODUCT_DEFINITION('Pin_03','Pin_03',#2295,#2278);
#2287=PRODUCT_DEFINITION('Base','Base',#2296,#2278);
#2288=PRODUCT_DEFINITION_FORMATION('',$,#2309);
#2289=PRODUCT_DEFINITION_FORMATION('',$,#2310);
#2290=PRODUCT_DEFINITION_FORMATION('',$,#2311);
#2291=PRODUCT_DEFINITION_FORMATION('',$,#2312);
#2292=PRODUCT_DEFINITION_FORMATION('',$,#2313);
#2293=PRODUCT_DEFINITION_FORMATION('',$,#2314);
#2294=PRODUCT_DEFINITION_FORMATION('',$,#2315);
#2295=PRODUCT_DEFINITION_FORMATION('',$,#2316);
#2296=PRODUCT_DEFINITION_FORMATION('',$,#2317);
#2297=PRODUCT_RELATED_PRODUCT_CATEGORY('BR-052','BR-052',(#2309));
#2298=PRODUCT_RELATED_PRODUCT_CATEGORY('Wheel','Wheel',(#2310));
#2299=PRODUCT_RELATED_PRODUCT_CATEGORY('Pin_01','Pin_01',(#2311));
#2300=PRODUCT_RELATED_PRODUCT_CATEGORY('Pin_02','Pin_02',(#2312));
#2301=PRODUCT_RELATED_PRODUCT_CATEGORY('Crank_01','Crank_01',(#2313));
#2302=PRODUCT_RELATED_PRODUCT_CATEGORY('Spacer','Spacer',(#2314));
#2303=PRODUCT_RELATED_PRODUCT_CATEGORY('Crank_02','Crank_02',(#2315));
#2304=PRODUCT_RELATED_PRODUCT_CATEGORY('Pin_03','Pin_03',(#2316));
#2305=PRODUCT_RELATED_PRODUCT_CATEGORY('Base','Base',(#2317));
#2306=APPLICATION_PROTOCOL_DEFINITION('international standard',
'automotive_design',2009,#2307);
#2307=APPLICATION_CONTEXT(
'Core Data for Automotive Mechanical Design Process');
#2308=PRODUCT_CONTEXT('part definition',#2307,'mechanical');
#2309=PRODUCT('BR-052','BR-052',$,(#2308));
#2310=PRODUCT('Wheel','Wheel',$,(#2308));
#2311=PRODUCT('Pin_01','Pin_01',$,(#2308));
#2312=PRODUCT('Pin_02','Pin_02',$,(#2308));
#2313=PRODUCT('Crank_01','Crank_01',$,(#2308));
#2314=PRODUCT('Spacer','Spacer',$,(#2308));
#2315=PRODUCT('Crank_02','Crank_02',$,(#2308));
#2316=PRODUCT('Pin_03','Pin_03',$,(#2308));
#2317=PRODUCT('Base','Base',$,(#2308));
#2318=PRESENTATION_STYLE_ASSIGNMENT((#2322));
#2319=PRESENTATION_STYLE_ASSIGNMENT((#2323));
#2320=PRESENTATION_STYLE_ASSIGNMENT((#2324));
#2321=PRESENTATION_STYLE_ASSIGNMENT((#2325));
#2322=SURFACE_STYLE_USAGE(.BOTH.,#2326);
#2323=SURFACE_STYLE_USAGE(.BOTH.,#2327);
#2324=SURFACE_STYLE_USAGE(.BOTH.,#2328);
#2325=SURFACE_STYLE_USAGE(.BOTH.,#2329);
#2326=SURFACE_SIDE_STYLE('',(#2330));
#2327=SURFACE_SIDE_STYLE('',(#2331));
#2328=SURFACE_SIDE_STYLE('',(#2332));
#2329=SURFACE_SIDE_STYLE('',(#2333));
#2330=SURFACE_STYLE_FILL_AREA(#2334);
#2331=SURFACE_STYLE_FILL_AREA(#2335);
#2332=SURFACE_STYLE_FILL_AREA(#2336);
#2333=SURFACE_STYLE_FILL_AREA(#2337);
#2334=FILL_AREA_STYLE('Steel - Satin',(#2338));
#2335=FILL_AREA_STYLE('Surface - Matte',(#2339));
#2336=FILL_AREA_STYLE('Surface - Matte',(#2340));
#2337=FILL_AREA_STYLE('Surface - Matte',(#2341));
#2338=FILL_AREA_STYLE_COLOUR('Steel - Satin',#2342);
#2339=FILL_AREA_STYLE_COLOUR('Surface - Matte',#2343);
#2340=FILL_AREA_STYLE_COLOUR('Surface - Matte',#2344);
#2341=FILL_AREA_STYLE_COLOUR('Surface - Matte',#2345);
#2342=COLOUR_RGB('Steel - Satin', 0.09019608, 0.27058824, 0.51372549);
#2343=COLOUR_RGB('Surface - Matte', 0.09019608, 0.27058824, 0.51372549);
#2344=COLOUR_RGB('Surface - Matte', 0.66274510, 0.83137255, 0.94901961);
#2345=COLOUR_RGB('Surface - Matte', 0.31764706, 0.68627451, 0.89019608);
ENDSEC;
END-ISO-10303-21;
